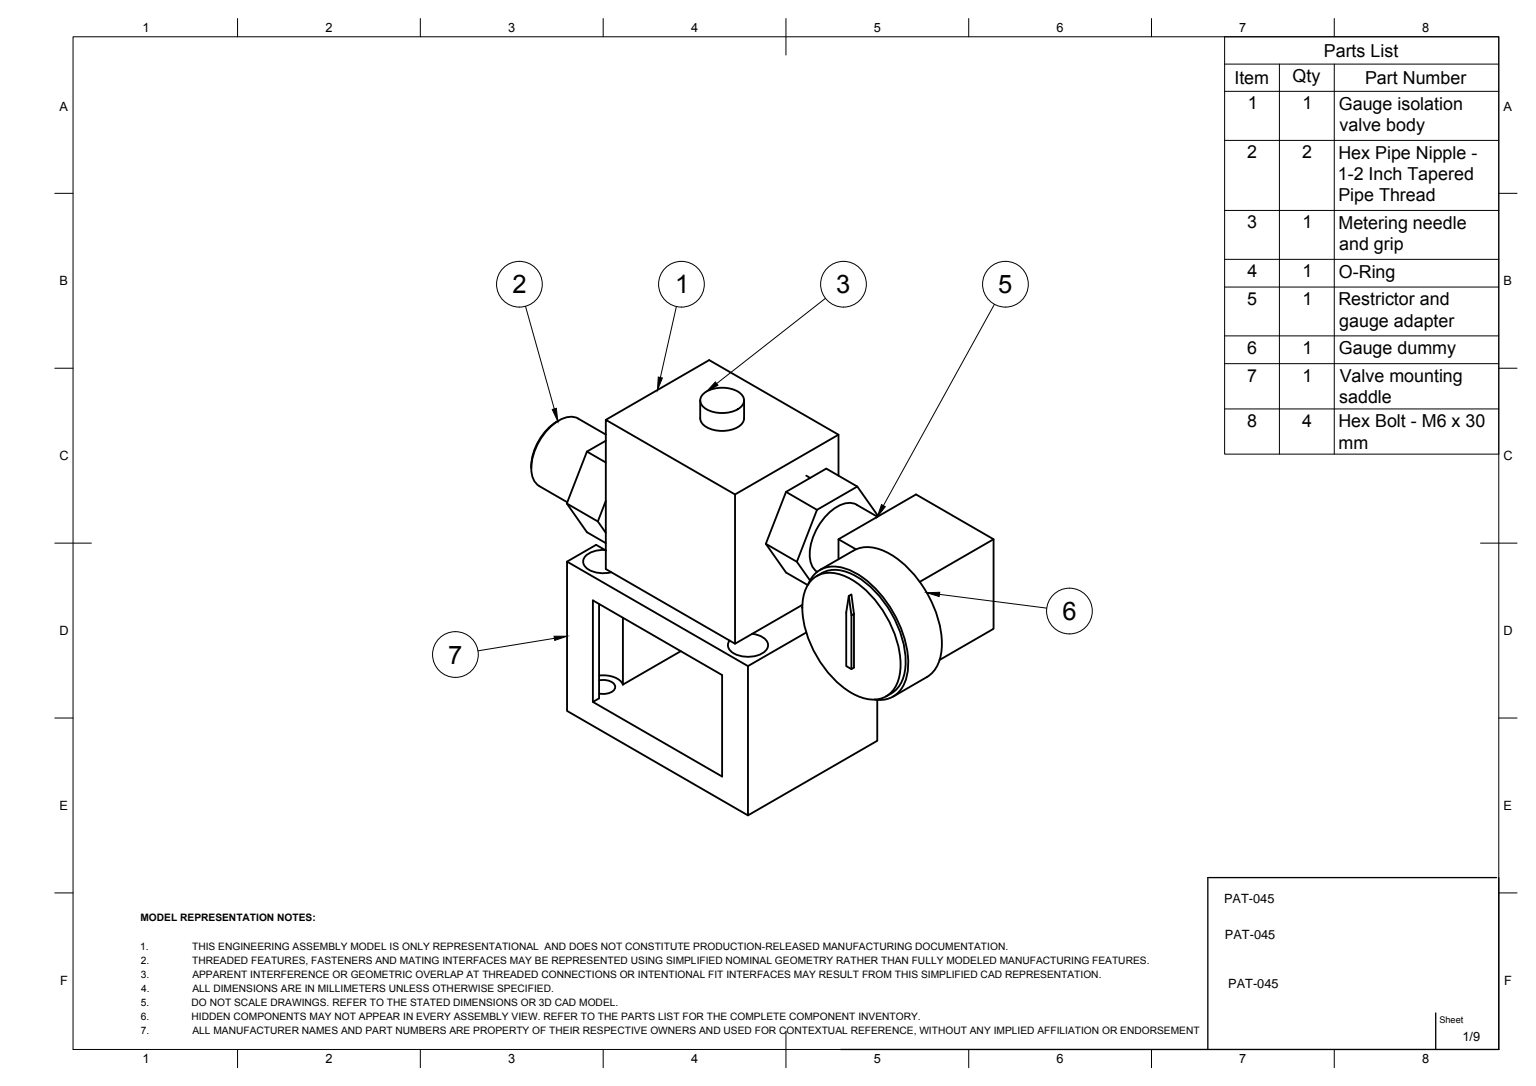
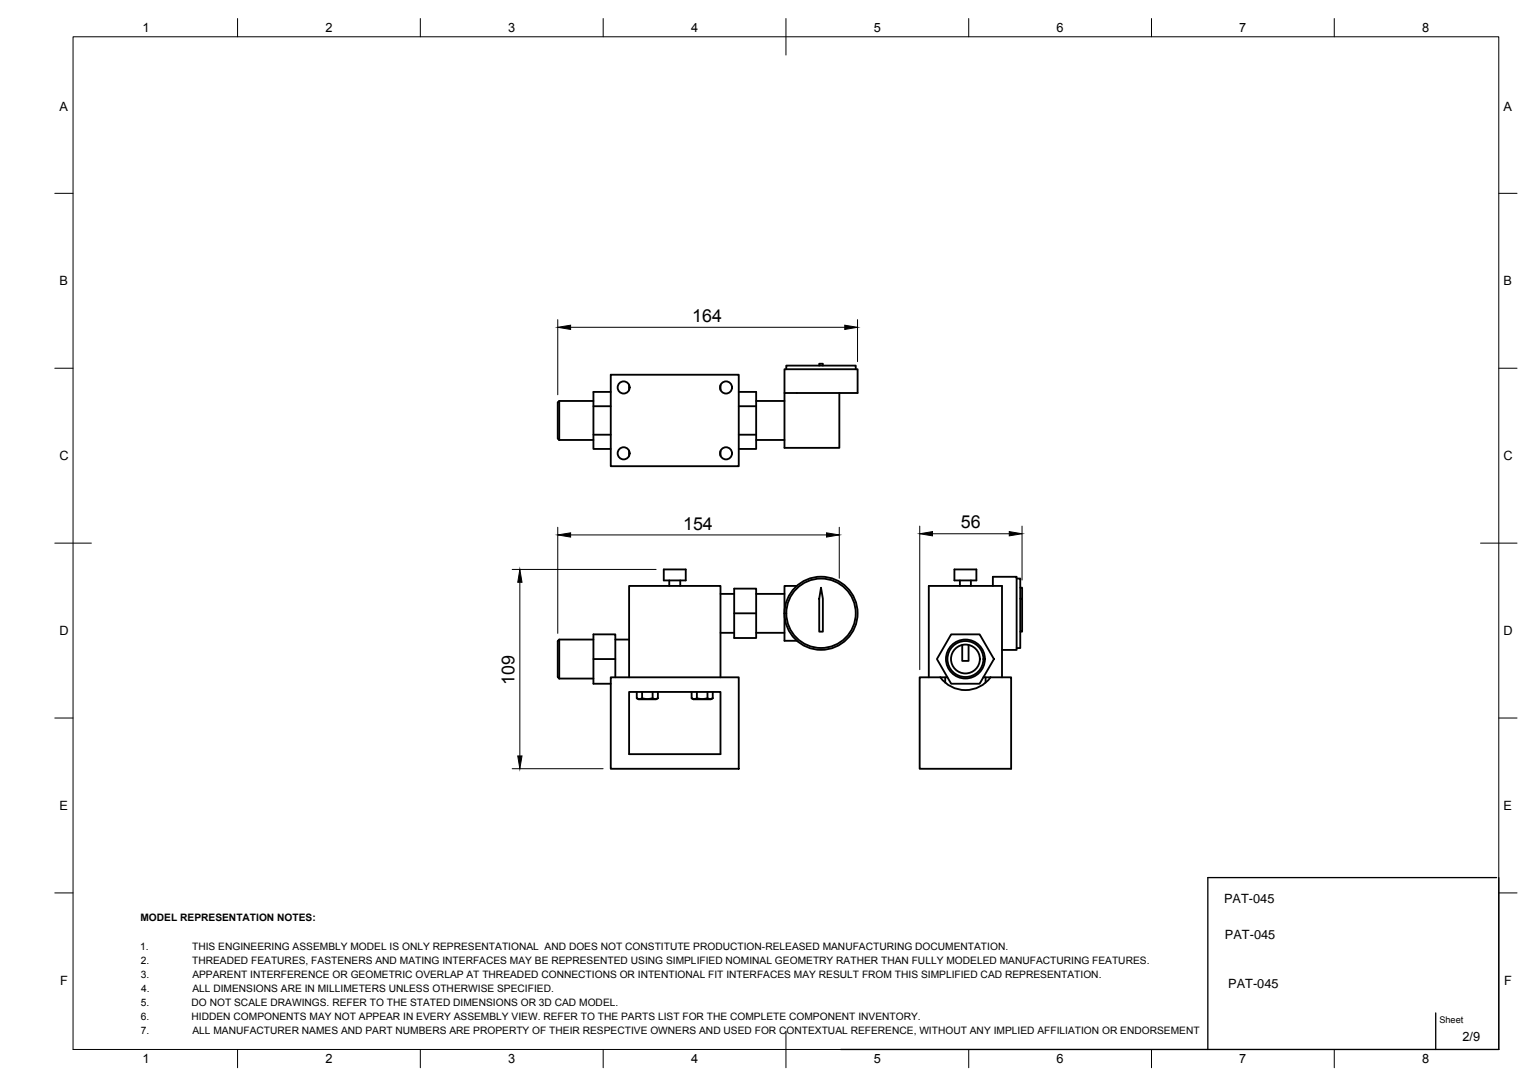
ISO-10303-21;
HEADER;
/* Generated by software containing ST-Developer
 * from STEP Tools, Inc. (www.steptools.com) 
 */

FILE_DESCRIPTION(
/* description */ ('Gauge isolation and snubber set'),
/* implementation_level */ '2;1');

FILE_NAME(
/* name */ 'PAT-045',
/* time_stamp */ '2026-10-29T16:58:15-07:00',
/* author */ (''),
/* organization */ (''),
/* preprocessor_version */ 'ST-DEVELOPER v20.2',
/* originating_system */ 'Autodesk Translation Framework v15.17.0.0',
/* authorisation */ '');

FILE_SCHEMA (('AUTOMOTIVE_DESIGN { 1 0 10303 214 3 1 1 }'));
ENDSEC;

DATA;
#10=MECHANICAL_DESIGN_GEOMETRIC_PRESENTATION_REPRESENTATION('',(#92,#93,
#94,#95,#96,#97,#98,#99,#100,#101),#4043);
#11=ITEM_DEFINED_TRANSFORMATION($,$,#2310,#2546);
#12=ITEM_DEFINED_TRANSFORMATION($,$,#2379,#2547);
#13=ITEM_DEFINED_TRANSFORMATION($,$,#2400,#2548);
#14=ITEM_DEFINED_TRANSFORMATION($,$,#2467,#2549);
#15=ITEM_DEFINED_TRANSFORMATION($,$,#2467,#2550);
#16=ITEM_DEFINED_TRANSFORMATION($,$,#2491,#2551);
#17=ITEM_DEFINED_TRANSFORMATION($,$,#2503,#2552);
#18=ITEM_DEFINED_TRANSFORMATION($,$,#2507,#2553);
#19=ITEM_DEFINED_TRANSFORMATION($,$,#2529,#2554);
#20=ITEM_DEFINED_TRANSFORMATION($,$,#2529,#2555);
#21=ITEM_DEFINED_TRANSFORMATION($,$,#2529,#2556);
#22=ITEM_DEFINED_TRANSFORMATION($,$,#2529,#2557);
#23=ITEM_DEFINED_TRANSFORMATION($,$,#2309,#2558);
#24=(
REPRESENTATION_RELATIONSHIP($,$,#4083,#4082)
REPRESENTATION_RELATIONSHIP_WITH_TRANSFORMATION(#11)
SHAPE_REPRESENTATION_RELATIONSHIP()
);
#25=(
REPRESENTATION_RELATIONSHIP($,$,#4084,#4082)
REPRESENTATION_RELATIONSHIP_WITH_TRANSFORMATION(#12)
SHAPE_REPRESENTATION_RELATIONSHIP()
);
#26=(
REPRESENTATION_RELATIONSHIP($,$,#4085,#4082)
REPRESENTATION_RELATIONSHIP_WITH_TRANSFORMATION(#13)
SHAPE_REPRESENTATION_RELATIONSHIP()
);
#27=(
REPRESENTATION_RELATIONSHIP($,$,#4086,#4082)
REPRESENTATION_RELATIONSHIP_WITH_TRANSFORMATION(#14)
SHAPE_REPRESENTATION_RELATIONSHIP()
);
#28=(
REPRESENTATION_RELATIONSHIP($,$,#4086,#4082)
REPRESENTATION_RELATIONSHIP_WITH_TRANSFORMATION(#15)
SHAPE_REPRESENTATION_RELATIONSHIP()
);
#29=(
REPRESENTATION_RELATIONSHIP($,$,#4087,#4082)
REPRESENTATION_RELATIONSHIP_WITH_TRANSFORMATION(#16)
SHAPE_REPRESENTATION_RELATIONSHIP()
);
#30=(
REPRESENTATION_RELATIONSHIP($,$,#4088,#4082)
REPRESENTATION_RELATIONSHIP_WITH_TRANSFORMATION(#17)
SHAPE_REPRESENTATION_RELATIONSHIP()
);
#31=(
REPRESENTATION_RELATIONSHIP($,$,#4089,#4082)
REPRESENTATION_RELATIONSHIP_WITH_TRANSFORMATION(#18)
SHAPE_REPRESENTATION_RELATIONSHIP()
);
#32=(
REPRESENTATION_RELATIONSHIP($,$,#4090,#4082)
REPRESENTATION_RELATIONSHIP_WITH_TRANSFORMATION(#19)
SHAPE_REPRESENTATION_RELATIONSHIP()
);
#33=(
REPRESENTATION_RELATIONSHIP($,$,#4090,#4082)
REPRESENTATION_RELATIONSHIP_WITH_TRANSFORMATION(#20)
SHAPE_REPRESENTATION_RELATIONSHIP()
);
#34=(
REPRESENTATION_RELATIONSHIP($,$,#4090,#4082)
REPRESENTATION_RELATIONSHIP_WITH_TRANSFORMATION(#21)
SHAPE_REPRESENTATION_RELATIONSHIP()
);
#35=(
REPRESENTATION_RELATIONSHIP($,$,#4090,#4082)
REPRESENTATION_RELATIONSHIP_WITH_TRANSFORMATION(#22)
SHAPE_REPRESENTATION_RELATIONSHIP()
);
#36=(
REPRESENTATION_RELATIONSHIP($,$,#4082,#4081)
REPRESENTATION_RELATIONSHIP_WITH_TRANSFORMATION(#23)
SHAPE_REPRESENTATION_RELATIONSHIP()
);
#37=CONTEXT_DEPENDENT_SHAPE_REPRESENTATION(#24,#4068);
#38=CONTEXT_DEPENDENT_SHAPE_REPRESENTATION(#25,#4069);
#39=CONTEXT_DEPENDENT_SHAPE_REPRESENTATION(#26,#4070);
#40=CONTEXT_DEPENDENT_SHAPE_REPRESENTATION(#27,#4071);
#41=CONTEXT_DEPENDENT_SHAPE_REPRESENTATION(#28,#4072);
#42=CONTEXT_DEPENDENT_SHAPE_REPRESENTATION(#29,#4073);
#43=CONTEXT_DEPENDENT_SHAPE_REPRESENTATION(#30,#4074);
#44=CONTEXT_DEPENDENT_SHAPE_REPRESENTATION(#31,#4075);
#45=CONTEXT_DEPENDENT_SHAPE_REPRESENTATION(#32,#4076);
#46=CONTEXT_DEPENDENT_SHAPE_REPRESENTATION(#33,#4077);
#47=CONTEXT_DEPENDENT_SHAPE_REPRESENTATION(#34,#4078);
#48=CONTEXT_DEPENDENT_SHAPE_REPRESENTATION(#35,#4079);
#49=CONTEXT_DEPENDENT_SHAPE_REPRESENTATION(#36,#4080);
#50=NEXT_ASSEMBLY_USAGE_OCCURRENCE('Gauge isolation valve body:1',
'Gauge isolation valve body:1','Gauge isolation valve body:1',#4093,#4094,
'Gauge isolation valve body:1');
#51=NEXT_ASSEMBLY_USAGE_OCCURRENCE('Restrictor and gauge adapter:1',
'Restrictor and gauge adapter:1','Restrictor and gauge adapter:1',#4093,
#4095,'Restrictor and gauge adapter:1');
#52=NEXT_ASSEMBLY_USAGE_OCCURRENCE('Valve mounting saddle:1',
'Valve mounting saddle:1','Valve mounting saddle:1',#4093,#4096,
'Valve mounting saddle:1');
#53=NEXT_ASSEMBLY_USAGE_OCCURRENCE(
'Hex Pipe Nipple - 1-2 Inch Tapered Pipe Thread:2',
'Hex Pipe Nipple - 1-2 Inch Tapered Pipe Thread:2',
'Hex Pipe Nipple - 1-2 Inch Tapered Pipe Thread:2',#4093,#4097,
'Hex Pipe Nipple - 1-2 Inch Tapered Pipe Thread:2');
#54=NEXT_ASSEMBLY_USAGE_OCCURRENCE(
'Hex Pipe Nipple - 1-2 Inch Tapered Pipe Thread:3',
'Hex Pipe Nipple - 1-2 Inch Tapered Pipe Thread:3',
'Hex Pipe Nipple - 1-2 Inch Tapered Pipe Thread:3',#4093,#4097,
'Hex Pipe Nipple - 1-2 Inch Tapered Pipe Thread:3');
#55=NEXT_ASSEMBLY_USAGE_OCCURRENCE('Metering needle and grip:2',
'Metering needle and grip:2','Metering needle and grip:2',#4093,#4098,
'Metering needle and grip:2');
#56=NEXT_ASSEMBLY_USAGE_OCCURRENCE('O-Ring:2','O-Ring:2','O-Ring:2',#4093,
#4099,'O-Ring:2');
#57=NEXT_ASSEMBLY_USAGE_OCCURRENCE('Gauge dummy:2','Gauge dummy:2',
'Gauge dummy:2',#4093,#4100,'Gauge dummy:2');
#58=NEXT_ASSEMBLY_USAGE_OCCURRENCE('Hex Bolt - M6 x 30 mm:2',
'Hex Bolt - M6 x 30 mm:2','Hex Bolt - M6 x 30 mm:2',#4093,#4101,
'Hex Bolt - M6 x 30 mm:2');
#59=NEXT_ASSEMBLY_USAGE_OCCURRENCE('Hex Bolt - M6 x 30 mm:3',
'Hex Bolt - M6 x 30 mm:3','Hex Bolt - M6 x 30 mm:3',#4093,#4101,
'Hex Bolt - M6 x 30 mm:3');
#60=NEXT_ASSEMBLY_USAGE_OCCURRENCE('Hex Bolt - M6 x 30 mm:4',
'Hex Bolt - M6 x 30 mm:4','Hex Bolt - M6 x 30 mm:4',#4093,#4101,
'Hex Bolt - M6 x 30 mm:4');
#61=NEXT_ASSEMBLY_USAGE_OCCURRENCE('Hex Bolt - M6 x 30 mm:5',
'Hex Bolt - M6 x 30 mm:5','Hex Bolt - M6 x 30 mm:5',#4093,#4101,
'Hex Bolt - M6 x 30 mm:5');
#62=NEXT_ASSEMBLY_USAGE_OCCURRENCE('Guage isolation set:1',
'Guage isolation set:1','Guage isolation set:1',#4092,#4093,
'Guage isolation set:1');
#63=(
BOUNDED_CURVE()
B_SPLINE_CURVE(2,(#3961,#3962,#3963),.UNSPECIFIED.,.F.,.F.)
B_SPLINE_CURVE_WITH_KNOTS((3,3),(0.144988513094728,0.791574906712449),
 .UNSPECIFIED.)
CURVE()
GEOMETRIC_REPRESENTATION_ITEM()
RATIONAL_B_SPLINE_CURVE((1.09282032302755,1.26188021535082,1.09282032302931))
REPRESENTATION_ITEM('')
);
#64=(
BOUNDED_CURVE()
B_SPLINE_CURVE(2,(#3965,#3966,#3967),.UNSPECIFIED.,.F.,.F.)
B_SPLINE_CURVE_WITH_KNOTS((3,3),(0.144988513094728,0.791574906712449),
 .UNSPECIFIED.)
CURVE()
GEOMETRIC_REPRESENTATION_ITEM()
RATIONAL_B_SPLINE_CURVE((1.09282032302755,1.26188021535082,1.09282032302931))
REPRESENTATION_ITEM('')
);
#65=(
BOUNDED_CURVE()
B_SPLINE_CURVE(2,(#3969,#3970,#3971),.UNSPECIFIED.,.F.,.F.)
B_SPLINE_CURVE_WITH_KNOTS((3,3),(0.144988513094728,0.791574906712449),
 .UNSPECIFIED.)
CURVE()
GEOMETRIC_REPRESENTATION_ITEM()
RATIONAL_B_SPLINE_CURVE((1.09282032302755,1.26188021535082,1.09282032302931))
REPRESENTATION_ITEM('')
);
#66=(
BOUNDED_CURVE()
B_SPLINE_CURVE(2,(#3973,#3974,#3975),.UNSPECIFIED.,.F.,.F.)
B_SPLINE_CURVE_WITH_KNOTS((3,3),(0.144988513094728,0.791574906712449),
 .UNSPECIFIED.)
CURVE()
GEOMETRIC_REPRESENTATION_ITEM()
RATIONAL_B_SPLINE_CURVE((1.09282032302755,1.26188021535082,1.09282032302931))
REPRESENTATION_ITEM('')
);
#67=(
BOUNDED_CURVE()
B_SPLINE_CURVE(2,(#3977,#3978,#3979),.UNSPECIFIED.,.F.,.F.)
B_SPLINE_CURVE_WITH_KNOTS((3,3),(0.144988513094728,0.791574906712449),
 .UNSPECIFIED.)
CURVE()
GEOMETRIC_REPRESENTATION_ITEM()
RATIONAL_B_SPLINE_CURVE((1.09282032302755,1.26188021535082,1.09282032302931))
REPRESENTATION_ITEM('')
);
#68=(
BOUNDED_CURVE()
B_SPLINE_CURVE(2,(#3980,#3981,#3982),.UNSPECIFIED.,.F.,.F.)
B_SPLINE_CURVE_WITH_KNOTS((3,3),(0.144988513094727,0.791574906712449),
 .UNSPECIFIED.)
CURVE()
GEOMETRIC_REPRESENTATION_ITEM()
RATIONAL_B_SPLINE_CURVE((1.09282032302755,1.26188021535082,1.09282032302931))
REPRESENTATION_ITEM('')
);
#69=TOROIDAL_SURFACE('',#2504,0.3925,0.089);
#70=CONICAL_SURFACE('',#2483,1.025,0.785398163397448);
#71=CONICAL_SURFACE('',#2486,1.025,0.785398163397448);
#72=CONICAL_SURFACE('',#2492,0.1,0.78539816339745);
#73=CONICAL_SURFACE('',#2494,0.25,0.321750554396641);
#74=CONICAL_SURFACE('',#2533,0.27,0.785398163397448);
#75=CONICAL_SURFACE('',#2536,0.576175134594813,1.0471975511966);
#76=SHAPE_REPRESENTATION_RELATIONSHIP('SRR','None',#4083,#84);
#77=SHAPE_REPRESENTATION_RELATIONSHIP('SRR','None',#4084,#85);
#78=SHAPE_REPRESENTATION_RELATIONSHIP('SRR','None',#4085,#86);
#79=SHAPE_REPRESENTATION_RELATIONSHIP('SRR','None',#4086,#87);
#80=SHAPE_REPRESENTATION_RELATIONSHIP('SRR','None',#4087,#88);
#81=SHAPE_REPRESENTATION_RELATIONSHIP('SRR','None',#4088,#89);
#82=SHAPE_REPRESENTATION_RELATIONSHIP('SRR','None',#4089,#90);
#83=SHAPE_REPRESENTATION_RELATIONSHIP('SRR','None',#4090,#91);
#84=ADVANCED_BREP_SHAPE_REPRESENTATION('',(#102),#4035);
#85=ADVANCED_BREP_SHAPE_REPRESENTATION('',(#103),#4036);
#86=ADVANCED_BREP_SHAPE_REPRESENTATION('',(#104),#4037);
#87=ADVANCED_BREP_SHAPE_REPRESENTATION('',(#105),#4038);
#88=ADVANCED_BREP_SHAPE_REPRESENTATION('',(#106),#4039);
#89=ADVANCED_BREP_SHAPE_REPRESENTATION('',(#107),#4040);
#90=ADVANCED_BREP_SHAPE_REPRESENTATION('',(#108,#109,#110),#4041);
#91=ADVANCED_BREP_SHAPE_REPRESENTATION('',(#111),#4042);
#92=STYLED_ITEM('',(#4176),#102);
#93=STYLED_ITEM('',(#4183),#103);
#94=STYLED_ITEM('',(#4211),#104);
#95=STYLED_ITEM('',(#4183),#105);
#96=STYLED_ITEM('',(#4204),#106);
#97=STYLED_ITEM('',(#4204),#107);
#98=STYLED_ITEM('',(#4211),#108);
#99=STYLED_ITEM('',(#4211),#109);
#100=STYLED_ITEM('',(#4211),#110);
#101=STYLED_ITEM('',(#4204),#111);
#102=MANIFOLD_SOLID_BREP('Body1',#2209);
#103=MANIFOLD_SOLID_BREP('Body1',#2210);
#104=MANIFOLD_SOLID_BREP('Body1',#2211);
#105=MANIFOLD_SOLID_BREP('Body1',#2212);
#106=MANIFOLD_SOLID_BREP('Body1',#2213);
#107=MANIFOLD_SOLID_BREP('Body1',#2214);
#108=MANIFOLD_SOLID_BREP('Body1',#2215);
#109=MANIFOLD_SOLID_BREP('Off white dial',#2216);
#110=MANIFOLD_SOLID_BREP('Black pointer',#2217);
#111=MANIFOLD_SOLID_BREP('Body1',#2218);
#112=FACE_BOUND('',#379,.T.);
#113=FACE_BOUND('',#382,.T.);
#114=FACE_BOUND('',#384,.T.);
#115=FACE_BOUND('',#389,.T.);
#116=FACE_BOUND('',#397,.T.);
#117=FACE_BOUND('',#400,.T.);
#118=FACE_BOUND('',#403,.T.);
#119=FACE_BOUND('',#405,.T.);
#120=FACE_BOUND('',#407,.T.);
#121=FACE_BOUND('',#408,.T.);
#122=FACE_BOUND('',#409,.T.);
#123=FACE_BOUND('',#410,.T.);
#124=FACE_BOUND('',#415,.T.);
#125=FACE_BOUND('',#419,.T.);
#126=FACE_BOUND('',#423,.T.);
#127=FACE_BOUND('',#425,.T.);
#128=FACE_BOUND('',#436,.T.);
#129=FACE_BOUND('',#437,.T.);
#130=FACE_BOUND('',#438,.T.);
#131=FACE_BOUND('',#439,.T.);
#132=FACE_BOUND('',#442,.T.);
#133=FACE_BOUND('',#443,.T.);
#134=FACE_BOUND('',#444,.T.);
#135=FACE_BOUND('',#445,.T.);
#136=FACE_BOUND('',#460,.T.);
#137=FACE_BOUND('',#462,.T.);
#138=FACE_BOUND('',#463,.T.);
#139=FACE_BOUND('',#464,.T.);
#140=FACE_BOUND('',#465,.T.);
#141=FACE_BOUND('',#467,.T.);
#142=FACE_BOUND('',#470,.T.);
#143=FACE_BOUND('',#471,.T.);
#144=FACE_BOUND('',#472,.T.);
#145=FACE_BOUND('',#473,.T.);
#146=FACE_BOUND('',#475,.T.);
#147=FACE_BOUND('',#477,.T.);
#148=FACE_BOUND('',#486,.T.);
#149=FACE_BOUND('',#491,.T.);
#150=FACE_BOUND('',#497,.T.);
#151=FACE_BOUND('',#502,.T.);
#152=FACE_BOUND('',#529,.T.);
#153=B_SPLINE_CURVE_WITH_KNOTS('',3,(#3286,#3287,#3288,#3289,#3290,#3291,
#3292,#3293,#3294,#3295,#3296,#3297,#3298,#3299,#3300,#3301,#3302,#3303),
 .UNSPECIFIED.,.F.,.F.,(4,2,2,2,2,2,2,2,4),(0.,0.0769830401762947,0.153966080352589,
0.230739261017803,0.307512441683016,0.384285622348229,0.461058803013443,
0.538041843189737,0.615024883366032),.UNSPECIFIED.);
#154=B_SPLINE_CURVE_WITH_KNOTS('',3,(#3360,#3361,#3362,#3363,#3364,#3365,
#3366,#3367,#3368,#3369,#3370,#3371,#3372,#3373,#3374),.UNSPECIFIED.,.F.,
 .F.,(4,2,2,2,3,2,4),(-0.302773934408822,-0.227086024595877,-0.151398114782933,
-0.0756990573914662,0.,0.0756990573914663,0.1003787904191),
 .UNSPECIFIED.);
#155=B_SPLINE_CURVE_WITH_KNOTS('',3,(#3377,#3378,#3379,#3380,#3381,#3382,
#3383,#3384,#3385,#3386,#3387,#3388,#3389,#3390),.UNSPECIFIED.,.F.,.F.,
(4,2,2,2,2,2,4),(-0.705926659236745,-0.681246926209111,-0.605547868817645,
-0.529848811426178,-0.454149754034712,-0.378461844221767,-0.302773934408822),
 .UNSPECIFIED.);
#156=B_SPLINE_CURVE_WITH_KNOTS('',3,(#3445,#3446,#3447,#3448,#3449,#3450,
#3451,#3452,#3453,#3454),.UNSPECIFIED.,.F.,.F.,(4,2,2,2,4),(0.0753445150177796,
0.0847625796770749,0.0941806443363702,0.10359870843152,0.113016772526669),
 .UNSPECIFIED.);
#157=B_SPLINE_CURVE_WITH_KNOTS('',3,(#3456,#3457,#3458,#3459,#3460,#3461,
#3462,#3463,#3464,#3465),.UNSPECIFIED.,.F.,.F.,(4,2,2,2,4),(0.0376722575088898,
0.0470903216040394,0.056508385699189,0.0659264503584843,0.0753445150177796),
 .UNSPECIFIED.);
#158=B_SPLINE_CURVE_WITH_KNOTS('',3,(#3470,#3471,#3472,#3473,#3474,#3475,
#3476,#3477,#3478,#3479),.UNSPECIFIED.,.F.,.F.,(4,2,2,2,4),(0.,0.0094180646592953,
0.0188361293185906,0.0282541934137402,0.0376722575088898),.UNSPECIFIED.);
#159=B_SPLINE_CURVE_WITH_KNOTS('',3,(#3480,#3481,#3482,#3483,#3484,#3485,
#3486,#3487,#3488,#3489),.UNSPECIFIED.,.F.,.F.,(4,2,2,2,4),(0.113016772526669,
0.122434836621819,0.131852900716969,0.141270965376264,0.150689030035559),
 .UNSPECIFIED.);
#160=B_SPLINE_CURVE_WITH_KNOTS('',3,(#3540,#3541,#3542,#3543,#3544,#3545,
#3546,#3547,#3548,#3549,#3550,#3551,#3552,#3553,#3554,#3555,#3556,#3557,
#3558,#3559),.UNSPECIFIED.,.F.,.F.,(4,2,2,2,2,2,2,2,2,4),(2.69569624904958,
2.75192095998156,2.89158432667083,3.02781992201341,3.15222641361202,3.27663290521063,
3.40103939680924,3.52544588840784,3.66168148375042,3.68881758098469),
 .UNSPECIFIED.);
#161=B_SPLINE_CURVE_WITH_KNOTS('',3,(#3563,#3564,#3565,#3566,#3567,#3568,
#3569,#3570,#3571,#3572,#3573,#3574,#3575,#3576),.UNSPECIFIED.,.F.,.F.,
(4,2,2,2,2,2,4),(2.49458037721665,2.67223802177451,2.78657360475194,2.90090918772936,
3.01524477070679,3.12958035368422,3.30723799824207),.UNSPECIFIED.);
#162=B_SPLINE_CURVE_WITH_KNOTS('',3,(#3584,#3585,#3586,#3587,#3588,#3589,
#3590,#3591,#3592,#3593,#3594,#3595,#3596,#3597,#3598),.UNSPECIFIED.,.F.,
 .F.,(4,2,2,3,2,2,4),(-0.40632881051271,-0.228671165954853,-0.114335582977427,
0.,0.114335582977426,0.228671165954853,0.40632881051271),.UNSPECIFIED.);
#163=B_SPLINE_CURVE_WITH_KNOTS('',3,(#3601,#3602,#3603,#3604,#3605,#3606,
#3607,#3608,#3609,#3610,#3611,#3612,#3613,#3614,#3615,#3616,#3617,#3618,
#3619,#3620,#3621),.UNSPECIFIED.,.F.,.F.,(4,2,2,2,3,2,2,2,2,4),(-0.412184675816244,
-0.385048578539797,-0.248812983197217,-0.124406491598609,0.,0.124406491598609,
0.248812983197217,0.385048578539798,0.524711945229068,0.58093665616105),
 .UNSPECIFIED.);
#164=PLANE('',#2319);
#165=PLANE('',#2323);
#166=PLANE('',#2327);
#167=PLANE('',#2331);
#168=PLANE('',#2332);
#169=PLANE('',#2339);
#170=PLANE('',#2343);
#171=PLANE('',#2347);
#172=PLANE('',#2349);
#173=PLANE('',#2358);
#174=PLANE('',#2359);
#175=PLANE('',#2362);
#176=PLANE('',#2365);
#177=PLANE('',#2372);
#178=PLANE('',#2373);
#179=PLANE('',#2374);
#180=PLANE('',#2375);
#181=PLANE('',#2376);
#182=PLANE('',#2377);
#183=PLANE('',#2378);
#184=PLANE('',#2383);
#185=PLANE('',#2387);
#186=PLANE('',#2393);
#187=PLANE('',#2394);
#188=PLANE('',#2395);
#189=PLANE('',#2396);
#190=PLANE('',#2397);
#191=PLANE('',#2398);
#192=PLANE('',#2399);
#193=PLANE('',#2401);
#194=PLANE('',#2424);
#195=PLANE('',#2425);
#196=PLANE('',#2435);
#197=PLANE('',#2443);
#198=PLANE('',#2446);
#199=PLANE('',#2447);
#200=PLANE('',#2450);
#201=PLANE('',#2456);
#202=PLANE('',#2461);
#203=PLANE('',#2462);
#204=PLANE('',#2463);
#205=PLANE('',#2464);
#206=PLANE('',#2465);
#207=PLANE('',#2466);
#208=PLANE('',#2468);
#209=PLANE('',#2470);
#210=PLANE('',#2472);
#211=PLANE('',#2473);
#212=PLANE('',#2474);
#213=PLANE('',#2475);
#214=PLANE('',#2476);
#215=PLANE('',#2477);
#216=PLANE('',#2480);
#217=PLANE('',#2488);
#218=PLANE('',#2498);
#219=PLANE('',#2502);
#220=PLANE('',#2508);
#221=PLANE('',#2513);
#222=PLANE('',#2516);
#223=PLANE('',#2520);
#224=PLANE('',#2521);
#225=PLANE('',#2522);
#226=PLANE('',#2523);
#227=PLANE('',#2524);
#228=PLANE('',#2525);
#229=PLANE('',#2526);
#230=PLANE('',#2527);
#231=PLANE('',#2528);
#232=PLANE('',#2535);
#233=PLANE('',#2538);
#234=PLANE('',#2539);
#235=PLANE('',#2540);
#236=PLANE('',#2541);
#237=PLANE('',#2542);
#238=PLANE('',#2543);
#239=PLANE('',#2544);
#240=PLANE('',#2545);
#241=FACE_OUTER_BOUND('',#365,.T.);
#242=FACE_OUTER_BOUND('',#366,.T.);
#243=FACE_OUTER_BOUND('',#367,.T.);
#244=FACE_OUTER_BOUND('',#368,.T.);
#245=FACE_OUTER_BOUND('',#369,.T.);
#246=FACE_OUTER_BOUND('',#370,.T.);
#247=FACE_OUTER_BOUND('',#371,.T.);
#248=FACE_OUTER_BOUND('',#372,.T.);
#249=FACE_OUTER_BOUND('',#373,.T.);
#250=FACE_OUTER_BOUND('',#374,.T.);
#251=FACE_OUTER_BOUND('',#375,.T.);
#252=FACE_OUTER_BOUND('',#376,.T.);
#253=FACE_OUTER_BOUND('',#377,.T.);
#254=FACE_OUTER_BOUND('',#378,.T.);
#255=FACE_OUTER_BOUND('',#380,.T.);
#256=FACE_OUTER_BOUND('',#381,.T.);
#257=FACE_OUTER_BOUND('',#383,.T.);
#258=FACE_OUTER_BOUND('',#385,.T.);
#259=FACE_OUTER_BOUND('',#386,.T.);
#260=FACE_OUTER_BOUND('',#387,.T.);
#261=FACE_OUTER_BOUND('',#388,.T.);
#262=FACE_OUTER_BOUND('',#390,.T.);
#263=FACE_OUTER_BOUND('',#391,.T.);
#264=FACE_OUTER_BOUND('',#392,.T.);
#265=FACE_OUTER_BOUND('',#393,.T.);
#266=FACE_OUTER_BOUND('',#394,.T.);
#267=FACE_OUTER_BOUND('',#395,.T.);
#268=FACE_OUTER_BOUND('',#396,.T.);
#269=FACE_OUTER_BOUND('',#398,.T.);
#270=FACE_OUTER_BOUND('',#399,.T.);
#271=FACE_OUTER_BOUND('',#401,.T.);
#272=FACE_OUTER_BOUND('',#402,.T.);
#273=FACE_OUTER_BOUND('',#404,.T.);
#274=FACE_OUTER_BOUND('',#406,.T.);
#275=FACE_OUTER_BOUND('',#411,.T.);
#276=FACE_OUTER_BOUND('',#412,.T.);
#277=FACE_OUTER_BOUND('',#413,.T.);
#278=FACE_OUTER_BOUND('',#414,.T.);
#279=FACE_OUTER_BOUND('',#416,.T.);
#280=FACE_OUTER_BOUND('',#417,.T.);
#281=FACE_OUTER_BOUND('',#418,.T.);
#282=FACE_OUTER_BOUND('',#420,.T.);
#283=FACE_OUTER_BOUND('',#421,.T.);
#284=FACE_OUTER_BOUND('',#422,.T.);
#285=FACE_OUTER_BOUND('',#424,.T.);
#286=FACE_OUTER_BOUND('',#426,.T.);
#287=FACE_OUTER_BOUND('',#427,.T.);
#288=FACE_OUTER_BOUND('',#428,.T.);
#289=FACE_OUTER_BOUND('',#429,.T.);
#290=FACE_OUTER_BOUND('',#430,.T.);
#291=FACE_OUTER_BOUND('',#431,.T.);
#292=FACE_OUTER_BOUND('',#432,.T.);
#293=FACE_OUTER_BOUND('',#433,.T.);
#294=FACE_OUTER_BOUND('',#434,.T.);
#295=FACE_OUTER_BOUND('',#435,.T.);
#296=FACE_OUTER_BOUND('',#440,.T.);
#297=FACE_OUTER_BOUND('',#441,.T.);
#298=FACE_OUTER_BOUND('',#446,.T.);
#299=FACE_OUTER_BOUND('',#447,.T.);
#300=FACE_OUTER_BOUND('',#448,.T.);
#301=FACE_OUTER_BOUND('',#449,.T.);
#302=FACE_OUTER_BOUND('',#450,.T.);
#303=FACE_OUTER_BOUND('',#451,.T.);
#304=FACE_OUTER_BOUND('',#452,.T.);
#305=FACE_OUTER_BOUND('',#453,.T.);
#306=FACE_OUTER_BOUND('',#454,.T.);
#307=FACE_OUTER_BOUND('',#455,.T.);
#308=FACE_OUTER_BOUND('',#456,.T.);
#309=FACE_OUTER_BOUND('',#457,.T.);
#310=FACE_OUTER_BOUND('',#458,.T.);
#311=FACE_OUTER_BOUND('',#459,.T.);
#312=FACE_OUTER_BOUND('',#461,.T.);
#313=FACE_OUTER_BOUND('',#466,.T.);
#314=FACE_OUTER_BOUND('',#468,.T.);
#315=FACE_OUTER_BOUND('',#469,.T.);
#316=FACE_OUTER_BOUND('',#474,.T.);
#317=FACE_OUTER_BOUND('',#476,.T.);
#318=FACE_OUTER_BOUND('',#478,.T.);
#319=FACE_OUTER_BOUND('',#479,.T.);
#320=FACE_OUTER_BOUND('',#480,.T.);
#321=FACE_OUTER_BOUND('',#481,.T.);
#322=FACE_OUTER_BOUND('',#482,.T.);
#323=FACE_OUTER_BOUND('',#483,.T.);
#324=FACE_OUTER_BOUND('',#484,.T.);
#325=FACE_OUTER_BOUND('',#485,.T.);
#326=FACE_OUTER_BOUND('',#487,.T.);
#327=FACE_OUTER_BOUND('',#488,.T.);
#328=FACE_OUTER_BOUND('',#489,.T.);
#329=FACE_OUTER_BOUND('',#490,.T.);
#330=FACE_OUTER_BOUND('',#492,.T.);
#331=FACE_OUTER_BOUND('',#493,.T.);
#332=FACE_OUTER_BOUND('',#494,.T.);
#333=FACE_OUTER_BOUND('',#495,.T.);
#334=FACE_OUTER_BOUND('',#496,.T.);
#335=FACE_OUTER_BOUND('',#498,.T.);
#336=FACE_OUTER_BOUND('',#499,.T.);
#337=FACE_OUTER_BOUND('',#500,.T.);
#338=FACE_OUTER_BOUND('',#501,.T.);
#339=FACE_OUTER_BOUND('',#503,.T.);
#340=FACE_OUTER_BOUND('',#504,.T.);
#341=FACE_OUTER_BOUND('',#505,.T.);
#342=FACE_OUTER_BOUND('',#506,.T.);
#343=FACE_OUTER_BOUND('',#507,.T.);
#344=FACE_OUTER_BOUND('',#508,.T.);
#345=FACE_OUTER_BOUND('',#509,.T.);
#346=FACE_OUTER_BOUND('',#510,.T.);
#347=FACE_OUTER_BOUND('',#511,.T.);
#348=FACE_OUTER_BOUND('',#512,.T.);
#349=FACE_OUTER_BOUND('',#513,.T.);
#350=FACE_OUTER_BOUND('',#514,.T.);
#351=FACE_OUTER_BOUND('',#515,.T.);
#352=FACE_OUTER_BOUND('',#516,.T.);
#353=FACE_OUTER_BOUND('',#517,.T.);
#354=FACE_OUTER_BOUND('',#518,.T.);
#355=FACE_OUTER_BOUND('',#519,.T.);
#356=FACE_OUTER_BOUND('',#520,.T.);
#357=FACE_OUTER_BOUND('',#521,.T.);
#358=FACE_OUTER_BOUND('',#522,.T.);
#359=FACE_OUTER_BOUND('',#523,.T.);
#360=FACE_OUTER_BOUND('',#524,.T.);
#361=FACE_OUTER_BOUND('',#525,.T.);
#362=FACE_OUTER_BOUND('',#526,.T.);
#363=FACE_OUTER_BOUND('',#527,.T.);
#364=FACE_OUTER_BOUND('',#528,.T.);
#365=EDGE_LOOP('',(#1461,#1462,#1463,#1464,#1465));
#366=EDGE_LOOP('',(#1466,#1467,#1468,#1469));
#367=EDGE_LOOP('',(#1470));
#368=EDGE_LOOP('',(#1471,#1472,#1473,#1474));
#369=EDGE_LOOP('',(#1475));
#370=EDGE_LOOP('',(#1476,#1477,#1478,#1479));
#371=EDGE_LOOP('',(#1480));
#372=EDGE_LOOP('',(#1481,#1482,#1483,#1484));
#373=EDGE_LOOP('',(#1485));
#374=EDGE_LOOP('',(#1486,#1487,#1488));
#375=EDGE_LOOP('',(#1489,#1490,#1491,#1492,#1493,#1494,#1495,#1496,#1497,
#1498,#1499,#1500));
#376=EDGE_LOOP('',(#1501,#1502,#1503));
#377=EDGE_LOOP('',(#1504,#1505,#1506,#1507));
#378=EDGE_LOOP('',(#1508));
#379=EDGE_LOOP('',(#1509));
#380=EDGE_LOOP('',(#1510,#1511,#1512,#1513));
#381=EDGE_LOOP('',(#1514));
#382=EDGE_LOOP('',(#1515));
#383=EDGE_LOOP('',(#1516));
#384=EDGE_LOOP('',(#1517));
#385=EDGE_LOOP('',(#1518,#1519,#1520,#1521));
#386=EDGE_LOOP('',(#1522,#1523,#1524,#1525));
#387=EDGE_LOOP('',(#1526,#1527,#1528,#1529,#1530));
#388=EDGE_LOOP('',(#1531,#1532));
#389=EDGE_LOOP('',(#1533));
#390=EDGE_LOOP('',(#1534,#1535,#1536,#1537,#1538,#1539,#1540,#1541));
#391=EDGE_LOOP('',(#1542,#1543));
#392=EDGE_LOOP('',(#1544,#1545,#1546,#1547,#1548,#1549,#1550,#1551,#1552,
#1553,#1554,#1555));
#393=EDGE_LOOP('',(#1556,#1557,#1558,#1559));
#394=EDGE_LOOP('',(#1560,#1561,#1562,#1563,#1564,#1565));
#395=EDGE_LOOP('',(#1566,#1567,#1568,#1569));
#396=EDGE_LOOP('',(#1570));
#397=EDGE_LOOP('',(#1571));
#398=EDGE_LOOP('',(#1572,#1573,#1574,#1575));
#399=EDGE_LOOP('',(#1576,#1577,#1578,#1579));
#400=EDGE_LOOP('',(#1580));
#401=EDGE_LOOP('',(#1581,#1582,#1583,#1584));
#402=EDGE_LOOP('',(#1585,#1586,#1587,#1588));
#403=EDGE_LOOP('',(#1589));
#404=EDGE_LOOP('',(#1590,#1591,#1592,#1593));
#405=EDGE_LOOP('',(#1594));
#406=EDGE_LOOP('',(#1595,#1596,#1597,#1598));
#407=EDGE_LOOP('',(#1599));
#408=EDGE_LOOP('',(#1600));
#409=EDGE_LOOP('',(#1601));
#410=EDGE_LOOP('',(#1602));
#411=EDGE_LOOP('',(#1603,#1604,#1605,#1606));
#412=EDGE_LOOP('',(#1607));
#413=EDGE_LOOP('',(#1608,#1609,#1610,#1611,#1612,#1613,#1614,#1615,#1616,
#1617));
#414=EDGE_LOOP('',(#1618));
#415=EDGE_LOOP('',(#1619));
#416=EDGE_LOOP('',(#1620,#1621,#1622,#1623,#1624,#1625,#1626));
#417=EDGE_LOOP('',(#1627,#1628,#1629,#1630));
#418=EDGE_LOOP('',(#1631));
#419=EDGE_LOOP('',(#1632));
#420=EDGE_LOOP('',(#1633,#1634,#1635,#1636));
#421=EDGE_LOOP('',(#1637,#1638,#1639,#1640));
#422=EDGE_LOOP('',(#1641,#1642,#1643,#1644));
#423=EDGE_LOOP('',(#1645));
#424=EDGE_LOOP('',(#1646,#1647,#1648,#1649));
#425=EDGE_LOOP('',(#1650));
#426=EDGE_LOOP('',(#1651,#1652,#1653,#1654));
#427=EDGE_LOOP('',(#1655,#1656,#1657,#1658));
#428=EDGE_LOOP('',(#1659,#1660,#1661,#1662));
#429=EDGE_LOOP('',(#1663,#1664,#1665,#1666,#1667,#1668,#1669,#1670,#1671,
#1672));
#430=EDGE_LOOP('',(#1673,#1674,#1675,#1676,#1677,#1678,#1679,#1680,#1681,
#1682));
#431=EDGE_LOOP('',(#1683,#1684,#1685,#1686,#1687,#1688,#1689));
#432=EDGE_LOOP('',(#1690,#1691,#1692,#1693,#1694,#1695,#1696));
#433=EDGE_LOOP('',(#1697,#1698,#1699,#1700,#1701,#1702,#1703,#1704));
#434=EDGE_LOOP('',(#1705,#1706,#1707,#1708));
#435=EDGE_LOOP('',(#1709,#1710,#1711,#1712,#1713,#1714,#1715,#1716,#1717,
#1718,#1719,#1720,#1721,#1722));
#436=EDGE_LOOP('',(#1723));
#437=EDGE_LOOP('',(#1724));
#438=EDGE_LOOP('',(#1725));
#439=EDGE_LOOP('',(#1726));
#440=EDGE_LOOP('',(#1727,#1728,#1729,#1730));
#441=EDGE_LOOP('',(#1731,#1732,#1733,#1734,#1735,#1736,#1737,#1738,#1739,
#1740,#1741,#1742,#1743,#1744));
#442=EDGE_LOOP('',(#1745));
#443=EDGE_LOOP('',(#1746));
#444=EDGE_LOOP('',(#1747));
#445=EDGE_LOOP('',(#1748));
#446=EDGE_LOOP('',(#1749,#1750,#1751,#1752,#1753,#1754,#1755,#1756));
#447=EDGE_LOOP('',(#1757,#1758,#1759,#1760));
#448=EDGE_LOOP('',(#1761,#1762,#1763,#1764));
#449=EDGE_LOOP('',(#1765,#1766,#1767,#1768));
#450=EDGE_LOOP('',(#1769,#1770,#1771,#1772));
#451=EDGE_LOOP('',(#1773,#1774,#1775,#1776));
#452=EDGE_LOOP('',(#1777,#1778,#1779,#1780));
#453=EDGE_LOOP('',(#1781,#1782,#1783,#1784,#1785,#1786,#1787,#1788,#1789,
#1790));
#454=EDGE_LOOP('',(#1791,#1792,#1793,#1794));
#455=EDGE_LOOP('',(#1795,#1796,#1797,#1798));
#456=EDGE_LOOP('',(#1799,#1800,#1801,#1802));
#457=EDGE_LOOP('',(#1803,#1804,#1805,#1806));
#458=EDGE_LOOP('',(#1807,#1808,#1809,#1810));
#459=EDGE_LOOP('',(#1811,#1812,#1813,#1814));
#460=EDGE_LOOP('',(#1815,#1816,#1817,#1818));
#461=EDGE_LOOP('',(#1819,#1820,#1821,#1822,#1823,#1824,#1825,#1826,#1827,
#1828,#1829,#1830,#1831,#1832,#1833,#1834,#1835,#1836));
#462=EDGE_LOOP('',(#1837));
#463=EDGE_LOOP('',(#1838));
#464=EDGE_LOOP('',(#1839));
#465=EDGE_LOOP('',(#1840));
#466=EDGE_LOOP('',(#1841,#1842,#1843,#1844));
#467=EDGE_LOOP('',(#1845,#1846,#1847,#1848));
#468=EDGE_LOOP('',(#1849,#1850,#1851,#1852,#1853,#1854));
#469=EDGE_LOOP('',(#1855,#1856,#1857,#1858));
#470=EDGE_LOOP('',(#1859));
#471=EDGE_LOOP('',(#1860));
#472=EDGE_LOOP('',(#1861));
#473=EDGE_LOOP('',(#1862));
#474=EDGE_LOOP('',(#1863,#1864,#1865,#1866,#1867,#1868));
#475=EDGE_LOOP('',(#1869));
#476=EDGE_LOOP('',(#1870,#1871,#1872,#1873,#1874,#1875));
#477=EDGE_LOOP('',(#1876));
#478=EDGE_LOOP('',(#1877,#1878,#1879,#1880));
#479=EDGE_LOOP('',(#1881,#1882,#1883,#1884));
#480=EDGE_LOOP('',(#1885,#1886,#1887,#1888));
#481=EDGE_LOOP('',(#1889,#1890,#1891,#1892));
#482=EDGE_LOOP('',(#1893,#1894,#1895,#1896));
#483=EDGE_LOOP('',(#1897,#1898,#1899,#1900));
#484=EDGE_LOOP('',(#1901,#1902,#1903,#1904));
#485=EDGE_LOOP('',(#1905));
#486=EDGE_LOOP('',(#1906));
#487=EDGE_LOOP('',(#1907,#1908,#1909,#1910));
#488=EDGE_LOOP('',(#1911,#1912,#1913,#1914));
#489=EDGE_LOOP('',(#1915,#1916,#1917,#1918));
#490=EDGE_LOOP('',(#1919));
#491=EDGE_LOOP('',(#1920));
#492=EDGE_LOOP('',(#1921,#1922,#1923,#1924));
#493=EDGE_LOOP('',(#1925,#1926,#1927));
#494=EDGE_LOOP('',(#1928,#1929,#1930,#1931));
#495=EDGE_LOOP('',(#1932,#1933,#1934,#1935));
#496=EDGE_LOOP('',(#1936));
#497=EDGE_LOOP('',(#1937));
#498=EDGE_LOOP('',(#1938,#1939,#1940,#1941));
#499=EDGE_LOOP('',(#1942));
#500=EDGE_LOOP('',(#1943,#1944,#1945,#1946));
#501=EDGE_LOOP('',(#1947));
#502=EDGE_LOOP('',(#1948));
#503=EDGE_LOOP('',(#1949,#1950,#1951,#1952));
#504=EDGE_LOOP('',(#1953));
#505=EDGE_LOOP('',(#1954,#1955,#1956,#1957));
#506=EDGE_LOOP('',(#1958));
#507=EDGE_LOOP('',(#1959,#1960,#1961,#1962));
#508=EDGE_LOOP('',(#1963));
#509=EDGE_LOOP('',(#1964));
#510=EDGE_LOOP('',(#1965,#1966,#1967,#1968));
#511=EDGE_LOOP('',(#1969,#1970,#1971,#1972));
#512=EDGE_LOOP('',(#1973,#1974,#1975,#1976));
#513=EDGE_LOOP('',(#1977,#1978,#1979,#1980));
#514=EDGE_LOOP('',(#1981,#1982,#1983,#1984));
#515=EDGE_LOOP('',(#1985,#1986,#1987,#1988,#1989));
#516=EDGE_LOOP('',(#1990,#1991,#1992,#1993,#1994));
#517=EDGE_LOOP('',(#1995,#1996,#1997,#1998));
#518=EDGE_LOOP('',(#1999,#2000,#2001,#2002));
#519=EDGE_LOOP('',(#2003));
#520=EDGE_LOOP('',(#2004,#2005,#2006,#2007,#2008,#2009,#2010,#2011,#2012));
#521=EDGE_LOOP('',(#2013,#2014,#2015,#2016));
#522=EDGE_LOOP('',(#2017,#2018,#2019,#2020));
#523=EDGE_LOOP('',(#2021,#2022,#2023,#2024));
#524=EDGE_LOOP('',(#2025,#2026,#2027,#2028));
#525=EDGE_LOOP('',(#2029,#2030,#2031,#2032));
#526=EDGE_LOOP('',(#2033,#2034,#2035,#2036));
#527=EDGE_LOOP('',(#2037));
#528=EDGE_LOOP('',(#2038,#2039,#2040,#2041,#2042,#2043));
#529=EDGE_LOOP('',(#2044));
#530=ELLIPSE('',#2313,0.565685424949238,0.4);
#531=ELLIPSE('',#2314,0.565685424949238,0.4);
#532=ELLIPSE('',#2336,0.565685424949238,0.4);
#533=ELLIPSE('',#2337,0.565685424949238,0.4);
#534=CIRCLE('',#2312,0.4);
#535=CIRCLE('',#2315,0.4);
#536=CIRCLE('',#2317,0.25);
#537=CIRCLE('',#2318,0.25);
#538=CIRCLE('',#2321,0.25);
#539=CIRCLE('',#2322,0.25);
#540=CIRCLE('',#2325,0.25);
#541=CIRCLE('',#2326,0.25);
#542=CIRCLE('',#2329,0.25);
#543=CIRCLE('',#2330,0.25);
#544=CIRCLE('',#2333,0.4);
#545=CIRCLE('',#2335,0.4);
#546=CIRCLE('',#2338,0.4);
#547=CIRCLE('',#2341,0.93);
#548=CIRCLE('',#2342,0.93);
#549=CIRCLE('',#2345,0.49);
#550=CIRCLE('',#2346,0.49);
#551=CIRCLE('',#2348,0.25);
#552=CIRCLE('',#2350,0.25);
#553=CIRCLE('',#2352,0.25);
#554=CIRCLE('',#2354,0.25);
#555=CIRCLE('',#2356,0.4);
#556=CIRCLE('',#2357,0.4);
#557=CIRCLE('',#2360,0.2);
#558=CIRCLE('',#2361,0.2);
#559=CIRCLE('',#2363,0.2);
#560=CIRCLE('',#2366,0.79);
#561=CIRCLE('',#2368,0.79);
#562=CIRCLE('',#2370,0.93);
#563=CIRCLE('',#2371,0.93);
#564=CIRCLE('',#2381,0.199999999999999);
#565=CIRCLE('',#2382,0.199999999999999);
#566=CIRCLE('',#2385,0.685);
#567=CIRCLE('',#2386,0.685);
#568=CIRCLE('',#2389,0.0250000000000004);
#569=CIRCLE('',#2391,0.93);
#570=CIRCLE('',#2392,0.93);
#571=CIRCLE('',#2402,1.7);
#572=CIRCLE('',#2404,1.7);
#573=CIRCLE('',#2406,0.55);
#574=CIRCLE('',#2407,0.55);
#575=CIRCLE('',#2408,0.55);
#576=CIRCLE('',#2409,0.55);
#577=CIRCLE('',#2410,0.55);
#578=CIRCLE('',#2412,0.33);
#579=CIRCLE('',#2413,0.33);
#580=CIRCLE('',#2414,0.33);
#581=CIRCLE('',#2416,0.33);
#582=CIRCLE('',#2417,0.33);
#583=CIRCLE('',#2418,0.33);
#584=CIRCLE('',#2420,0.55);
#585=CIRCLE('',#2421,0.55);
#586=CIRCLE('',#2422,0.55);
#587=CIRCLE('',#2423,0.55);
#588=CIRCLE('',#2426,0.55);
#589=CIRCLE('',#2427,0.55);
#590=CIRCLE('',#2428,0.55);
#591=CIRCLE('',#2429,0.33);
#592=CIRCLE('',#2430,0.33);
#593=CIRCLE('',#2431,0.33);
#594=CIRCLE('',#2432,0.33);
#595=CIRCLE('',#2434,0.33);
#596=CIRCLE('',#2436,0.55);
#597=CIRCLE('',#2437,0.55);
#598=CIRCLE('',#2438,0.55);
#599=CIRCLE('',#2439,0.33);
#600=CIRCLE('',#2440,0.33);
#601=CIRCLE('',#2442,0.55);
#602=CIRCLE('',#2445,0.33);
#603=CIRCLE('',#2449,0.33);
#604=CIRCLE('',#2452,0.55);
#605=CIRCLE('',#2453,0.55);
#606=CIRCLE('',#2455,0.33);
#607=CIRCLE('',#2458,0.33);
#608=CIRCLE('',#2460,0.33);
#609=CIRCLE('',#2469,1.065);
#610=CIRCLE('',#2471,1.065);
#611=CIRCLE('',#2479,1.065);
#612=CIRCLE('',#2481,0.985);
#613=CIRCLE('',#2482,0.79);
#614=CIRCLE('',#2485,1.065);
#615=CIRCLE('',#2487,0.985);
#616=CIRCLE('',#2489,0.79);
#617=CIRCLE('',#2493,0.2);
#618=CIRCLE('',#2495,0.3);
#619=CIRCLE('',#2497,0.3);
#620=CIRCLE('',#2499,0.6);
#621=CIRCLE('',#2501,0.6);
#622=CIRCLE('',#2505,0.089);
#623=CIRCLE('',#2506,0.3035);
#624=CIRCLE('',#2509,2.);
#625=CIRCLE('',#2510,0.685);
#626=CIRCLE('',#2512,2.);
#627=CIRCLE('',#2515,0.685);
#628=CIRCLE('',#2518,1.9);
#629=CIRCLE('',#2519,1.9);
#630=CIRCLE('',#2531,0.2942);
#631=CIRCLE('',#2532,0.2942);
#632=CIRCLE('',#2534,0.24);
#633=CIRCLE('',#2537,0.475);
#634=LINE('',#3238,#805);
#635=LINE('',#3250,#806);
#636=LINE('',#3257,#807);
#637=LINE('',#3264,#808);
#638=LINE('',#3271,#809);
#639=LINE('',#3277,#810);
#640=LINE('',#3280,#811);
#641=LINE('',#3283,#812);
#642=LINE('',#3305,#813);
#643=LINE('',#3310,#814);
#644=LINE('',#3314,#815);
#645=LINE('',#3315,#816);
#646=LINE('',#3320,#817);
#647=LINE('',#3327,#818);
#648=LINE('',#3338,#819);
#649=LINE('',#3341,#820);
#650=LINE('',#3354,#821);
#651=LINE('',#3358,#822);
#652=LINE('',#3375,#823);
#653=LINE('',#3391,#824);
#654=LINE('',#3397,#825);
#655=LINE('',#3402,#826);
#656=LINE('',#3408,#827);
#657=LINE('',#3410,#828);
#658=LINE('',#3412,#829);
#659=LINE('',#3413,#830);
#660=LINE('',#3416,#831);
#661=LINE('',#3418,#832);
#662=LINE('',#3419,#833);
#663=LINE('',#3422,#834);
#664=LINE('',#3424,#835);
#665=LINE('',#3425,#836);
#666=LINE('',#3427,#837);
#667=LINE('',#3428,#838);
#668=LINE('',#3436,#839);
#669=LINE('',#3443,#840);
#670=LINE('',#3467,#841);
#671=LINE('',#3494,#842);
#672=LINE('',#3499,#843);
#673=LINE('',#3505,#844);
#674=LINE('',#3507,#845);
#675=LINE('',#3509,#846);
#676=LINE('',#3510,#847);
#677=LINE('',#3513,#848);
#678=LINE('',#3515,#849);
#679=LINE('',#3516,#850);
#680=LINE('',#3519,#851);
#681=LINE('',#3521,#852);
#682=LINE('',#3522,#853);
#683=LINE('',#3524,#854);
#684=LINE('',#3525,#855);
#685=LINE('',#3532,#856);
#686=LINE('',#3536,#857);
#687=LINE('',#3537,#858);
#688=LINE('',#3561,#859);
#689=LINE('',#3578,#860);
#690=LINE('',#3582,#861);
#691=LINE('',#3600,#862);
#692=LINE('',#3625,#863);
#693=LINE('',#3629,#864);
#694=LINE('',#3633,#865);
#695=LINE('',#3641,#866);
#696=LINE('',#3648,#867);
#697=LINE('',#3654,#868);
#698=LINE('',#3658,#869);
#699=LINE('',#3663,#870);
#700=LINE('',#3667,#871);
#701=LINE('',#3669,#872);
#702=LINE('',#3670,#873);
#703=LINE('',#3673,#874);
#704=LINE('',#3675,#875);
#705=LINE('',#3676,#876);
#706=LINE('',#3678,#877);
#707=LINE('',#3684,#878);
#708=LINE('',#3686,#879);
#709=LINE('',#3688,#880);
#710=LINE('',#3701,#881);
#711=LINE('',#3708,#882);
#712=LINE('',#3710,#883);
#713=LINE('',#3712,#884);
#714=LINE('',#3715,#885);
#715=LINE('',#3717,#886);
#716=LINE('',#3719,#887);
#717=LINE('',#3720,#888);
#718=LINE('',#3726,#889);
#719=LINE('',#3728,#890);
#720=LINE('',#3731,#891);
#721=LINE('',#3735,#892);
#722=LINE('',#3737,#893);
#723=LINE('',#3739,#894);
#724=LINE('',#3743,#895);
#725=LINE('',#3745,#896);
#726=LINE('',#3747,#897);
#727=LINE('',#3749,#898);
#728=LINE('',#3755,#899);
#729=LINE('',#3757,#900);
#730=LINE('',#3760,#901);
#731=LINE('',#3764,#902);
#732=LINE('',#3769,#903);
#733=LINE('',#3771,#904);
#734=LINE('',#3773,#905);
#735=LINE('',#3774,#906);
#736=LINE('',#3777,#907);
#737=LINE('',#3779,#908);
#738=LINE('',#3780,#909);
#739=LINE('',#3782,#910);
#740=LINE('',#3784,#911);
#741=LINE('',#3785,#912);
#742=LINE('',#3788,#913);
#743=LINE('',#3789,#914);
#744=LINE('',#3791,#915);
#745=LINE('',#3797,#916);
#746=LINE('',#3799,#917);
#747=LINE('',#3801,#918);
#748=LINE('',#3803,#919);
#749=LINE('',#3805,#920);
#750=LINE('',#3806,#921);
#751=LINE('',#3812,#922);
#752=LINE('',#3814,#923);
#753=LINE('',#3816,#924);
#754=LINE('',#3818,#925);
#755=LINE('',#3820,#926);
#756=LINE('',#3821,#927);
#757=LINE('',#3825,#928);
#758=LINE('',#3826,#929);
#759=LINE('',#3828,#930);
#760=LINE('',#3830,#931);
#761=LINE('',#3832,#932);
#762=LINE('',#3834,#933);
#763=LINE('',#3838,#934);
#764=LINE('',#3846,#935);
#765=LINE('',#3850,#936);
#766=LINE('',#3854,#937);
#767=LINE('',#3859,#938);
#768=LINE('',#3865,#939);
#769=LINE('',#3869,#940);
#770=LINE('',#3873,#941);
#771=LINE('',#3880,#942);
#772=LINE('',#3895,#943);
#773=LINE('',#3901,#944);
#774=LINE('',#3907,#945);
#775=LINE('',#3914,#946);
#776=LINE('',#3916,#947);
#777=LINE('',#3918,#948);
#778=LINE('',#3919,#949);
#779=LINE('',#3922,#950);
#780=LINE('',#3924,#951);
#781=LINE('',#3925,#952);
#782=LINE('',#3928,#953);
#783=LINE('',#3930,#954);
#784=LINE('',#3931,#955);
#785=LINE('',#3934,#956);
#786=LINE('',#3936,#957);
#787=LINE('',#3937,#958);
#788=LINE('',#3939,#959);
#789=LINE('',#3940,#960);
#790=LINE('',#3948,#961);
#791=LINE('',#3953,#962);
#792=LINE('',#3959,#963);
#793=LINE('',#3985,#964);
#794=LINE('',#3987,#965);
#795=LINE('',#3988,#966);
#796=LINE('',#3991,#967);
#797=LINE('',#3992,#968);
#798=LINE('',#3995,#969);
#799=LINE('',#3996,#970);
#800=LINE('',#3999,#971);
#801=LINE('',#4000,#972);
#802=LINE('',#4003,#973);
#803=LINE('',#4004,#974);
#804=LINE('',#4006,#975);
#805=VECTOR('',#2567,0.4);
#806=VECTOR('',#2580,0.25);
#807=VECTOR('',#2589,0.25);
#808=VECTOR('',#2598,0.25);
#809=VECTOR('',#2607,0.25);
#810=VECTOR('',#2614,1.);
#811=VECTOR('',#2617,1.);
#812=VECTOR('',#2620,1.);
#813=VECTOR('',#2623,1.);
#814=VECTOR('',#2628,0.4);
#815=VECTOR('',#2633,1.);
#816=VECTOR('',#2634,1.);
#817=VECTOR('',#2639,0.93);
#818=VECTOR('',#2648,0.49);
#819=VECTOR('',#2663,0.25);
#820=VECTOR('',#2666,0.25);
#821=VECTOR('',#2685,1.);
#822=VECTOR('',#2690,1.);
#823=VECTOR('',#2691,0.2);
#824=VECTOR('',#2692,1.);
#825=VECTOR('',#2701,0.79);
#826=VECTOR('',#2706,0.93);
#827=VECTOR('',#2713,1.);
#828=VECTOR('',#2714,1.);
#829=VECTOR('',#2715,1.);
#830=VECTOR('',#2716,1.);
#831=VECTOR('',#2719,1.);
#832=VECTOR('',#2720,1.);
#833=VECTOR('',#2721,1.);
#834=VECTOR('',#2724,1.);
#835=VECTOR('',#2725,1.);
#836=VECTOR('',#2726,1.);
#837=VECTOR('',#2729,1.);
#838=VECTOR('',#2730,1.);
#839=VECTOR('',#2741,0.199999999999999);
#840=VECTOR('',#2750,0.685);
#841=VECTOR('',#2751,0.685);
#842=VECTOR('',#2760,0.0250000000000004);
#843=VECTOR('',#2765,0.93);
#844=VECTOR('',#2772,1.);
#845=VECTOR('',#2773,1.);
#846=VECTOR('',#2774,1.);
#847=VECTOR('',#2775,1.);
#848=VECTOR('',#2778,1.);
#849=VECTOR('',#2779,1.);
#850=VECTOR('',#2780,1.);
#851=VECTOR('',#2783,1.);
#852=VECTOR('',#2784,1.);
#853=VECTOR('',#2785,1.);
#854=VECTOR('',#2788,1.);
#855=VECTOR('',#2789,1.);
#856=VECTOR('',#2798,1.);
#857=VECTOR('',#2801,1.);
#858=VECTOR('',#2802,1.);
#859=VECTOR('',#2805,1.);
#860=VECTOR('',#2806,1.);
#861=VECTOR('',#2809,1.);
#862=VECTOR('',#2810,1.);
#863=VECTOR('',#2813,1.);
#864=VECTOR('',#2816,1.);
#865=VECTOR('',#2819,0.55);
#866=VECTOR('',#2830,0.33);
#867=VECTOR('',#2839,0.33);
#868=VECTOR('',#2846,1.);
#869=VECTOR('',#2849,0.55);
#870=VECTOR('',#2854,1.);
#871=VECTOR('',#2859,1.);
#872=VECTOR('',#2860,1.);
#873=VECTOR('',#2861,1.);
#874=VECTOR('',#2864,1.);
#875=VECTOR('',#2865,1.);
#876=VECTOR('',#2866,1.);
#877=VECTOR('',#2867,1.);
#878=VECTOR('',#2872,1.);
#879=VECTOR('',#2873,1.);
#880=VECTOR('',#2874,1.);
#881=VECTOR('',#2889,0.33);
#882=VECTOR('',#2896,1.);
#883=VECTOR('',#2897,1.);
#884=VECTOR('',#2898,1.);
#885=VECTOR('',#2901,1.);
#886=VECTOR('',#2902,1.);
#887=VECTOR('',#2903,1.);
#888=VECTOR('',#2904,1.);
#889=VECTOR('',#2911,1.);
#890=VECTOR('',#2912,0.55);
#891=VECTOR('',#2917,1.);
#892=VECTOR('',#2922,0.33);
#893=VECTOR('',#2925,1.);
#894=VECTOR('',#2928,1.);
#895=VECTOR('',#2933,0.33);
#896=VECTOR('',#2936,1.);
#897=VECTOR('',#2939,1.);
#898=VECTOR('',#2940,0.55);
#899=VECTOR('',#2949,0.33);
#900=VECTOR('',#2952,1.);
#901=VECTOR('',#2955,0.33);
#902=VECTOR('',#2960,0.33);
#903=VECTOR('',#2965,1.);
#904=VECTOR('',#2966,1.);
#905=VECTOR('',#2967,1.);
#906=VECTOR('',#2968,1.);
#907=VECTOR('',#2971,1.);
#908=VECTOR('',#2972,1.);
#909=VECTOR('',#2973,1.);
#910=VECTOR('',#2976,1.);
#911=VECTOR('',#2977,1.);
#912=VECTOR('',#2978,1.);
#913=VECTOR('',#2981,1.);
#914=VECTOR('',#2982,1.);
#915=VECTOR('',#2985,1.);
#916=VECTOR('',#2992,1.);
#917=VECTOR('',#2993,1.);
#918=VECTOR('',#2994,1.);
#919=VECTOR('',#2995,1.);
#920=VECTOR('',#2996,1.);
#921=VECTOR('',#2997,1.);
#922=VECTOR('',#3002,1.);
#923=VECTOR('',#3003,1.);
#924=VECTOR('',#3004,1.);
#925=VECTOR('',#3005,1.);
#926=VECTOR('',#3006,1.);
#927=VECTOR('',#3007,1.);
#928=VECTOR('',#3012,1.);
#929=VECTOR('',#3013,1.);
#930=VECTOR('',#3016,1.);
#931=VECTOR('',#3019,1.);
#932=VECTOR('',#3022,1.);
#933=VECTOR('',#3025,1.);
#934=VECTOR('',#3030,1.065);
#935=VECTOR('',#3041,1.025);
#936=VECTOR('',#3046,1.065);
#937=VECTOR('',#3051,1.025);
#938=VECTOR('',#3058,0.79);
#939=VECTOR('',#3065,0.1);
#940=VECTOR('',#3070,0.25);
#941=VECTOR('',#3075,0.3);
#942=VECTOR('',#3084,0.6);
#943=VECTOR('',#3105,2.);
#944=VECTOR('',#3114,0.685);
#945=VECTOR('',#3121,1.9);
#946=VECTOR('',#3130,1.);
#947=VECTOR('',#3131,1.);
#948=VECTOR('',#3132,1.);
#949=VECTOR('',#3133,1.);
#950=VECTOR('',#3136,1.);
#951=VECTOR('',#3137,1.);
#952=VECTOR('',#3138,1.);
#953=VECTOR('',#3141,1.);
#954=VECTOR('',#3142,1.);
#955=VECTOR('',#3143,1.);
#956=VECTOR('',#3146,1.);
#957=VECTOR('',#3147,1.);
#958=VECTOR('',#3148,1.);
#959=VECTOR('',#3151,1.);
#960=VECTOR('',#3152,1.);
#961=VECTOR('',#3163,0.3);
#962=VECTOR('',#3170,0.27);
#963=VECTOR('',#3177,0.576175134594813);
#964=VECTOR('',#3180,1.);
#965=VECTOR('',#3181,1.);
#966=VECTOR('',#3182,1.);
#967=VECTOR('',#3185,1.);
#968=VECTOR('',#3186,1.);
#969=VECTOR('',#3189,1.);
#970=VECTOR('',#3190,1.);
#971=VECTOR('',#3193,1.);
#972=VECTOR('',#3194,1.);
#973=VECTOR('',#3197,1.);
#974=VECTOR('',#3198,1.);
#975=VECTOR('',#3201,1.);
#976=VERTEX_POINT('',#3236);
#977=VERTEX_POINT('',#3237);
#978=VERTEX_POINT('',#3239);
#979=VERTEX_POINT('',#3241);
#980=VERTEX_POINT('',#3243);
#981=VERTEX_POINT('',#3247);
#982=VERTEX_POINT('',#3249);
#983=VERTEX_POINT('',#3254);
#984=VERTEX_POINT('',#3256);
#985=VERTEX_POINT('',#3261);
#986=VERTEX_POINT('',#3263);
#987=VERTEX_POINT('',#3268);
#988=VERTEX_POINT('',#3270);
#989=VERTEX_POINT('',#3275);
#990=VERTEX_POINT('',#3276);
#991=VERTEX_POINT('',#3278);
#992=VERTEX_POINT('',#3282);
#993=VERTEX_POINT('',#3284);
#994=VERTEX_POINT('',#3304);
#995=VERTEX_POINT('',#3306);
#996=VERTEX_POINT('',#3309);
#997=VERTEX_POINT('',#3313);
#998=VERTEX_POINT('',#3317);
#999=VERTEX_POINT('',#3319);
#1000=VERTEX_POINT('',#3324);
#1001=VERTEX_POINT('',#3326);
#1002=VERTEX_POINT('',#3330);
#1003=VERTEX_POINT('',#3333);
#1004=VERTEX_POINT('',#3336);
#1005=VERTEX_POINT('',#3340);
#1006=VERTEX_POINT('',#3348);
#1007=VERTEX_POINT('',#3352);
#1008=VERTEX_POINT('',#3353);
#1009=VERTEX_POINT('',#3357);
#1010=VERTEX_POINT('',#3359);
#1011=VERTEX_POINT('',#3376);
#1012=VERTEX_POINT('',#3395);
#1013=VERTEX_POINT('',#3399);
#1014=VERTEX_POINT('',#3401);
#1015=VERTEX_POINT('',#3406);
#1016=VERTEX_POINT('',#3407);
#1017=VERTEX_POINT('',#3409);
#1018=VERTEX_POINT('',#3411);
#1019=VERTEX_POINT('',#3415);
#1020=VERTEX_POINT('',#3417);
#1021=VERTEX_POINT('',#3421);
#1022=VERTEX_POINT('',#3423);
#1023=VERTEX_POINT('',#3433);
#1024=VERTEX_POINT('',#3435);
#1025=VERTEX_POINT('',#3440);
#1026=VERTEX_POINT('',#3442);
#1027=VERTEX_POINT('',#3444);
#1028=VERTEX_POINT('',#3455);
#1029=VERTEX_POINT('',#3466);
#1030=VERTEX_POINT('',#3469);
#1031=VERTEX_POINT('',#3492);
#1032=VERTEX_POINT('',#3496);
#1033=VERTEX_POINT('',#3498);
#1034=VERTEX_POINT('',#3503);
#1035=VERTEX_POINT('',#3504);
#1036=VERTEX_POINT('',#3506);
#1037=VERTEX_POINT('',#3508);
#1038=VERTEX_POINT('',#3512);
#1039=VERTEX_POINT('',#3514);
#1040=VERTEX_POINT('',#3518);
#1041=VERTEX_POINT('',#3520);
#1042=VERTEX_POINT('',#3530);
#1043=VERTEX_POINT('',#3531);
#1044=VERTEX_POINT('',#3533);
#1045=VERTEX_POINT('',#3535);
#1046=VERTEX_POINT('',#3539);
#1047=VERTEX_POINT('',#3560);
#1048=VERTEX_POINT('',#3562);
#1049=VERTEX_POINT('',#3577);
#1050=VERTEX_POINT('',#3579);
#1051=VERTEX_POINT('',#3581);
#1052=VERTEX_POINT('',#3583);
#1053=VERTEX_POINT('',#3599);
#1054=VERTEX_POINT('',#3623);
#1055=VERTEX_POINT('',#3624);
#1056=VERTEX_POINT('',#3626);
#1057=VERTEX_POINT('',#3628);
#1058=VERTEX_POINT('',#3630);
#1059=VERTEX_POINT('',#3632);
#1060=VERTEX_POINT('',#3638);
#1061=VERTEX_POINT('',#3640);
#1062=VERTEX_POINT('',#3645);
#1063=VERTEX_POINT('',#3647);
#1064=VERTEX_POINT('',#3652);
#1065=VERTEX_POINT('',#3653);
#1066=VERTEX_POINT('',#3655);
#1067=VERTEX_POINT('',#3657);
#1068=VERTEX_POINT('',#3660);
#1069=VERTEX_POINT('',#3662);
#1070=VERTEX_POINT('',#3666);
#1071=VERTEX_POINT('',#3668);
#1072=VERTEX_POINT('',#3672);
#1073=VERTEX_POINT('',#3674);
#1074=VERTEX_POINT('',#3677);
#1075=VERTEX_POINT('',#3679);
#1076=VERTEX_POINT('',#3681);
#1077=VERTEX_POINT('',#3683);
#1078=VERTEX_POINT('',#3685);
#1079=VERTEX_POINT('',#3687);
#1080=VERTEX_POINT('',#3690);
#1081=VERTEX_POINT('',#3692);
#1082=VERTEX_POINT('',#3694);
#1083=VERTEX_POINT('',#3696);
#1084=VERTEX_POINT('',#3699);
#1085=VERTEX_POINT('',#3703);
#1086=VERTEX_POINT('',#3705);
#1087=VERTEX_POINT('',#3707);
#1088=VERTEX_POINT('',#3709);
#1089=VERTEX_POINT('',#3711);
#1090=VERTEX_POINT('',#3713);
#1091=VERTEX_POINT('',#3716);
#1092=VERTEX_POINT('',#3718);
#1093=VERTEX_POINT('',#3721);
#1094=VERTEX_POINT('',#3723);
#1095=VERTEX_POINT('',#3727);
#1096=VERTEX_POINT('',#3733);
#1097=VERTEX_POINT('',#3741);
#1098=VERTEX_POINT('',#3748);
#1099=VERTEX_POINT('',#3753);
#1100=VERTEX_POINT('',#3759);
#1101=VERTEX_POINT('',#3763);
#1102=VERTEX_POINT('',#3767);
#1103=VERTEX_POINT('',#3768);
#1104=VERTEX_POINT('',#3770);
#1105=VERTEX_POINT('',#3772);
#1106=VERTEX_POINT('',#3776);
#1107=VERTEX_POINT('',#3778);
#1108=VERTEX_POINT('',#3783);
#1109=VERTEX_POINT('',#3787);
#1110=VERTEX_POINT('',#3795);
#1111=VERTEX_POINT('',#3796);
#1112=VERTEX_POINT('',#3798);
#1113=VERTEX_POINT('',#3800);
#1114=VERTEX_POINT('',#3802);
#1115=VERTEX_POINT('',#3804);
#1116=VERTEX_POINT('',#3807);
#1117=VERTEX_POINT('',#3810);
#1118=VERTEX_POINT('',#3811);
#1119=VERTEX_POINT('',#3813);
#1120=VERTEX_POINT('',#3815);
#1121=VERTEX_POINT('',#3817);
#1122=VERTEX_POINT('',#3819);
#1123=VERTEX_POINT('',#3822);
#1124=VERTEX_POINT('',#3837);
#1125=VERTEX_POINT('',#3841);
#1126=VERTEX_POINT('',#3843);
#1127=VERTEX_POINT('',#3848);
#1128=VERTEX_POINT('',#3852);
#1129=VERTEX_POINT('',#3856);
#1130=VERTEX_POINT('',#3862);
#1131=VERTEX_POINT('',#3864);
#1132=VERTEX_POINT('',#3867);
#1133=VERTEX_POINT('',#3871);
#1134=VERTEX_POINT('',#3875);
#1135=VERTEX_POINT('',#3878);
#1136=VERTEX_POINT('',#3884);
#1137=VERTEX_POINT('',#3889);
#1138=VERTEX_POINT('',#3891);
#1139=VERTEX_POINT('',#3894);
#1140=VERTEX_POINT('',#3899);
#1141=VERTEX_POINT('',#3904);
#1142=VERTEX_POINT('',#3906);
#1143=VERTEX_POINT('',#3912);
#1144=VERTEX_POINT('',#3913);
#1145=VERTEX_POINT('',#3915);
#1146=VERTEX_POINT('',#3917);
#1147=VERTEX_POINT('',#3921);
#1148=VERTEX_POINT('',#3923);
#1149=VERTEX_POINT('',#3927);
#1150=VERTEX_POINT('',#3929);
#1151=VERTEX_POINT('',#3933);
#1152=VERTEX_POINT('',#3935);
#1153=VERTEX_POINT('',#3945);
#1154=VERTEX_POINT('',#3947);
#1155=VERTEX_POINT('',#3951);
#1156=VERTEX_POINT('',#3956);
#1157=VERTEX_POINT('',#3958);
#1158=VERTEX_POINT('',#3960);
#1159=VERTEX_POINT('',#3964);
#1160=VERTEX_POINT('',#3968);
#1161=VERTEX_POINT('',#3972);
#1162=VERTEX_POINT('',#3976);
#1163=VERTEX_POINT('',#3984);
#1164=VERTEX_POINT('',#3986);
#1165=VERTEX_POINT('',#3990);
#1166=VERTEX_POINT('',#3994);
#1167=VERTEX_POINT('',#3998);
#1168=VERTEX_POINT('',#4002);
#1169=EDGE_CURVE('',#976,#977,#634,.T.);
#1170=EDGE_CURVE('',#978,#976,#534,.T.);
#1171=EDGE_CURVE('',#978,#979,#530,.T.);
#1172=EDGE_CURVE('',#979,#980,#531,.T.);
#1173=EDGE_CURVE('',#980,#977,#535,.T.);
#1174=EDGE_CURVE('',#981,#981,#536,.T.);
#1175=EDGE_CURVE('',#981,#982,#635,.T.);
#1176=EDGE_CURVE('',#982,#982,#537,.T.);
#1177=EDGE_CURVE('',#983,#983,#538,.T.);
#1178=EDGE_CURVE('',#983,#984,#636,.T.);
#1179=EDGE_CURVE('',#984,#984,#539,.T.);
#1180=EDGE_CURVE('',#985,#985,#540,.T.);
#1181=EDGE_CURVE('',#985,#986,#637,.T.);
#1182=EDGE_CURVE('',#986,#986,#541,.T.);
#1183=EDGE_CURVE('',#987,#987,#542,.T.);
#1184=EDGE_CURVE('',#987,#988,#638,.T.);
#1185=EDGE_CURVE('',#988,#988,#543,.T.);
#1186=EDGE_CURVE('',#989,#990,#639,.T.);
#1187=EDGE_CURVE('',#989,#991,#544,.T.);
#1188=EDGE_CURVE('',#990,#991,#640,.T.);
#1189=EDGE_CURVE('',#992,#978,#641,.T.);
#1190=EDGE_CURVE('',#993,#992,#545,.T.);
#1191=EDGE_CURVE('',#991,#993,#153,.T.);
#1192=EDGE_CURVE('',#994,#989,#642,.T.);
#1193=EDGE_CURVE('',#995,#994,#532,.T.);
#1194=EDGE_CURVE('',#980,#995,#533,.T.);
#1195=EDGE_CURVE('',#980,#996,#643,.T.);
#1196=EDGE_CURVE('',#996,#996,#546,.T.);
#1197=EDGE_CURVE('',#997,#992,#644,.T.);
#1198=EDGE_CURVE('',#993,#997,#645,.T.);
#1199=EDGE_CURVE('',#998,#998,#547,.T.);
#1200=EDGE_CURVE('',#998,#999,#646,.T.);
#1201=EDGE_CURVE('',#999,#999,#548,.T.);
#1202=EDGE_CURVE('',#1000,#1000,#549,.T.);
#1203=EDGE_CURVE('',#1000,#1001,#647,.T.);
#1204=EDGE_CURVE('',#1001,#1001,#550,.T.);
#1205=EDGE_CURVE('',#1002,#1002,#551,.T.);
#1206=EDGE_CURVE('',#1003,#1003,#552,.T.);
#1207=EDGE_CURVE('',#1004,#1004,#553,.T.);
#1208=EDGE_CURVE('',#1004,#1003,#648,.T.);
#1209=EDGE_CURVE('',#1002,#1005,#649,.T.);
#1210=EDGE_CURVE('',#1005,#1005,#554,.T.);
#1211=EDGE_CURVE('',#977,#980,#555,.T.);
#1212=EDGE_CURVE('',#976,#994,#556,.T.);
#1213=EDGE_CURVE('',#1006,#990,#557,.T.);
#1214=EDGE_CURVE('',#997,#1006,#558,.T.);
#1215=EDGE_CURVE('',#1007,#1008,#650,.T.);
#1216=EDGE_CURVE('',#1007,#1008,#559,.T.);
#1217=EDGE_CURVE('',#1009,#1007,#651,.T.);
#1218=EDGE_CURVE('',#1010,#1009,#154,.T.);
#1219=EDGE_CURVE('',#1010,#1006,#652,.T.);
#1220=EDGE_CURVE('',#1011,#1010,#155,.T.);
#1221=EDGE_CURVE('',#1008,#1011,#653,.T.);
#1222=EDGE_CURVE('',#1009,#1011,#560,.T.);
#1223=EDGE_CURVE('',#1012,#1012,#561,.T.);
#1224=EDGE_CURVE('',#1012,#1010,#654,.T.);
#1225=EDGE_CURVE('',#1013,#1013,#562,.T.);
#1226=EDGE_CURVE('',#1013,#1014,#655,.T.);
#1227=EDGE_CURVE('',#1014,#1014,#563,.T.);
#1228=EDGE_CURVE('',#1015,#1016,#656,.T.);
#1229=EDGE_CURVE('',#1016,#1017,#657,.T.);
#1230=EDGE_CURVE('',#1018,#1017,#658,.T.);
#1231=EDGE_CURVE('',#1015,#1018,#659,.T.);
#1232=EDGE_CURVE('',#1019,#1015,#660,.T.);
#1233=EDGE_CURVE('',#1020,#1018,#661,.T.);
#1234=EDGE_CURVE('',#1019,#1020,#662,.T.);
#1235=EDGE_CURVE('',#1021,#1019,#663,.T.);
#1236=EDGE_CURVE('',#1022,#1020,#664,.T.);
#1237=EDGE_CURVE('',#1021,#1022,#665,.T.);
#1238=EDGE_CURVE('',#1016,#1021,#666,.T.);
#1239=EDGE_CURVE('',#1017,#1022,#667,.T.);
#1240=EDGE_CURVE('',#1023,#1023,#564,.T.);
#1241=EDGE_CURVE('',#1023,#1024,#668,.T.);
#1242=EDGE_CURVE('',#1024,#1024,#565,.T.);
#1243=EDGE_CURVE('',#1025,#1025,#566,.T.);
#1244=EDGE_CURVE('',#1025,#1026,#669,.T.);
#1245=EDGE_CURVE('',#1027,#1026,#156,.T.);
#1246=EDGE_CURVE('',#1028,#1027,#157,.T.);
#1247=EDGE_CURVE('',#1028,#1029,#670,.T.);
#1248=EDGE_CURVE('',#1029,#1029,#567,.T.);
#1249=EDGE_CURVE('',#1030,#1028,#158,.T.);
#1250=EDGE_CURVE('',#1026,#1030,#159,.T.);
#1251=EDGE_CURVE('',#1031,#1031,#568,.T.);
#1252=EDGE_CURVE('',#1031,#1027,#671,.T.);
#1253=EDGE_CURVE('',#1032,#1032,#569,.T.);
#1254=EDGE_CURVE('',#1032,#1033,#672,.T.);
#1255=EDGE_CURVE('',#1033,#1033,#570,.T.);
#1256=EDGE_CURVE('',#1034,#1035,#673,.T.);
#1257=EDGE_CURVE('',#1035,#1036,#674,.T.);
#1258=EDGE_CURVE('',#1037,#1036,#675,.T.);
#1259=EDGE_CURVE('',#1034,#1037,#676,.T.);
#1260=EDGE_CURVE('',#1038,#1034,#677,.T.);
#1261=EDGE_CURVE('',#1039,#1037,#678,.T.);
#1262=EDGE_CURVE('',#1038,#1039,#679,.T.);
#1263=EDGE_CURVE('',#1040,#1038,#680,.T.);
#1264=EDGE_CURVE('',#1041,#1039,#681,.T.);
#1265=EDGE_CURVE('',#1040,#1041,#682,.T.);
#1266=EDGE_CURVE('',#1035,#1040,#683,.T.);
#1267=EDGE_CURVE('',#1036,#1041,#684,.T.);
#1268=EDGE_CURVE('',#1042,#1043,#685,.T.);
#1269=EDGE_CURVE('',#1044,#1042,#571,.T.);
#1270=EDGE_CURVE('',#1045,#1044,#686,.T.);
#1271=EDGE_CURVE('',#1043,#1045,#687,.T.);
#1272=EDGE_CURVE('',#1046,#1042,#160,.T.);
#1273=EDGE_CURVE('',#1047,#1046,#688,.T.);
#1274=EDGE_CURVE('',#1048,#1047,#161,.T.);
#1275=EDGE_CURVE('',#1049,#1048,#689,.T.);
#1276=EDGE_CURVE('',#1050,#1049,#572,.T.);
#1277=EDGE_CURVE('',#1051,#1050,#690,.T.);
#1278=EDGE_CURVE('',#1052,#1051,#162,.T.);
#1279=EDGE_CURVE('',#1053,#1052,#691,.T.);
#1280=EDGE_CURVE('',#1044,#1053,#163,.T.);
#1281=EDGE_CURVE('',#1054,#1055,#692,.T.);
#1282=EDGE_CURVE('',#1056,#1054,#573,.T.);
#1283=EDGE_CURVE('',#1057,#1056,#693,.T.);
#1284=EDGE_CURVE('',#1058,#1057,#574,.T.);
#1285=EDGE_CURVE('',#1058,#1059,#694,.T.);
#1286=EDGE_CURVE('',#1048,#1059,#575,.T.);
#1287=EDGE_CURVE('',#1059,#1047,#576,.T.);
#1288=EDGE_CURVE('',#1055,#1058,#577,.T.);
#1289=EDGE_CURVE('',#1060,#1060,#578,.T.);
#1290=EDGE_CURVE('',#1060,#1061,#695,.T.);
#1291=EDGE_CURVE('',#1046,#1061,#579,.T.);
#1292=EDGE_CURVE('',#1061,#1043,#580,.T.);
#1293=EDGE_CURVE('',#1062,#1062,#581,.T.);
#1294=EDGE_CURVE('',#1062,#1063,#696,.T.);
#1295=EDGE_CURVE('',#1045,#1063,#582,.T.);
#1296=EDGE_CURVE('',#1063,#1053,#583,.T.);
#1297=EDGE_CURVE('',#1064,#1065,#697,.T.);
#1298=EDGE_CURVE('',#1066,#1064,#584,.T.);
#1299=EDGE_CURVE('',#1066,#1067,#698,.T.);
#1300=EDGE_CURVE('',#1067,#1067,#585,.T.);
#1301=EDGE_CURVE('',#1068,#1066,#586,.T.);
#1302=EDGE_CURVE('',#1069,#1068,#699,.T.);
#1303=EDGE_CURVE('',#1065,#1069,#587,.T.);
#1304=EDGE_CURVE('',#1070,#1065,#700,.T.);
#1305=EDGE_CURVE('',#1070,#1071,#701,.T.);
#1306=EDGE_CURVE('',#1071,#1064,#702,.T.);
#1307=EDGE_CURVE('',#1069,#1072,#703,.T.);
#1308=EDGE_CURVE('',#1072,#1073,#704,.T.);
#1309=EDGE_CURVE('',#1073,#1055,#705,.T.);
#1310=EDGE_CURVE('',#1057,#1074,#706,.T.);
#1311=EDGE_CURVE('',#1074,#1075,#588,.T.);
#1312=EDGE_CURVE('',#1075,#1076,#589,.T.);
#1313=EDGE_CURVE('',#1076,#1077,#707,.T.);
#1314=EDGE_CURVE('',#1077,#1078,#708,.T.);
#1315=EDGE_CURVE('',#1078,#1079,#709,.T.);
#1316=EDGE_CURVE('',#1079,#1070,#590,.T.);
#1317=EDGE_CURVE('',#1080,#1080,#591,.T.);
#1318=EDGE_CURVE('',#1081,#1081,#592,.T.);
#1319=EDGE_CURVE('',#1082,#1082,#593,.T.);
#1320=EDGE_CURVE('',#1083,#1083,#594,.T.);
#1321=EDGE_CURVE('',#1084,#1084,#595,.T.);
#1322=EDGE_CURVE('',#1084,#1083,#710,.T.);
#1323=EDGE_CURVE('',#1071,#1085,#596,.T.);
#1324=EDGE_CURVE('',#1085,#1086,#597,.T.);
#1325=EDGE_CURVE('',#1087,#1086,#711,.T.);
#1326=EDGE_CURVE('',#1088,#1087,#712,.T.);
#1327=EDGE_CURVE('',#1089,#1088,#713,.T.);
#1328=EDGE_CURVE('',#1089,#1090,#598,.T.);
#1329=EDGE_CURVE('',#1056,#1090,#714,.T.);
#1330=EDGE_CURVE('',#1091,#1054,#715,.T.);
#1331=EDGE_CURVE('',#1092,#1091,#716,.T.);
#1332=EDGE_CURVE('',#1068,#1092,#717,.T.);
#1333=EDGE_CURVE('',#1093,#1093,#599,.T.);
#1334=EDGE_CURVE('',#1094,#1094,#600,.T.);
#1335=EDGE_CURVE('',#1086,#1079,#718,.T.);
#1336=EDGE_CURVE('',#1085,#1095,#719,.T.);
#1337=EDGE_CURVE('',#1095,#1095,#601,.T.);
#1338=EDGE_CURVE('',#1087,#1078,#720,.T.);
#1339=EDGE_CURVE('',#1096,#1096,#602,.T.);
#1340=EDGE_CURVE('',#1096,#1080,#721,.T.);
#1341=EDGE_CURVE('',#1072,#1092,#722,.T.);
#1342=EDGE_CURVE('',#1073,#1091,#723,.T.);
#1343=EDGE_CURVE('',#1097,#1097,#603,.T.);
#1344=EDGE_CURVE('',#1097,#1082,#724,.T.);
#1345=EDGE_CURVE('',#1090,#1074,#725,.T.);
#1346=EDGE_CURVE('',#1076,#1089,#726,.T.);
#1347=EDGE_CURVE('',#1075,#1098,#727,.T.);
#1348=EDGE_CURVE('',#1052,#1098,#604,.T.);
#1349=EDGE_CURVE('',#1098,#1051,#605,.T.);
#1350=EDGE_CURVE('',#1099,#1099,#606,.T.);
#1351=EDGE_CURVE('',#1099,#1081,#728,.T.);
#1352=EDGE_CURVE('',#1088,#1077,#729,.T.);
#1353=EDGE_CURVE('',#1094,#1100,#730,.T.);
#1354=EDGE_CURVE('',#1100,#1100,#607,.T.);
#1355=EDGE_CURVE('',#1093,#1101,#731,.T.);
#1356=EDGE_CURVE('',#1101,#1101,#608,.T.);
#1357=EDGE_CURVE('',#1102,#1103,#732,.T.);
#1358=EDGE_CURVE('',#1102,#1104,#733,.T.);
#1359=EDGE_CURVE('',#1104,#1105,#734,.T.);
#1360=EDGE_CURVE('',#1105,#1103,#735,.T.);
#1361=EDGE_CURVE('',#1106,#1103,#736,.T.);
#1362=EDGE_CURVE('',#1107,#1106,#737,.T.);
#1363=EDGE_CURVE('',#1107,#1102,#738,.T.);
#1364=EDGE_CURVE('',#1050,#1106,#739,.T.);
#1365=EDGE_CURVE('',#1108,#1105,#740,.T.);
#1366=EDGE_CURVE('',#1108,#1049,#741,.T.);
#1367=EDGE_CURVE('',#1104,#1109,#742,.T.);
#1368=EDGE_CURVE('',#1109,#1108,#743,.T.);
#1369=EDGE_CURVE('',#1109,#1107,#744,.T.);
#1370=EDGE_CURVE('',#1110,#1111,#745,.T.);
#1371=EDGE_CURVE('',#1111,#1112,#746,.T.);
#1372=EDGE_CURVE('',#1112,#1113,#747,.T.);
#1373=EDGE_CURVE('',#1113,#1114,#748,.T.);
#1374=EDGE_CURVE('',#1114,#1115,#749,.T.);
#1375=EDGE_CURVE('',#1115,#1110,#750,.T.);
#1376=EDGE_CURVE('',#1116,#1116,#609,.T.);
#1377=EDGE_CURVE('',#1117,#1118,#751,.T.);
#1378=EDGE_CURVE('',#1118,#1119,#752,.T.);
#1379=EDGE_CURVE('',#1119,#1120,#753,.T.);
#1380=EDGE_CURVE('',#1120,#1121,#754,.T.);
#1381=EDGE_CURVE('',#1121,#1122,#755,.T.);
#1382=EDGE_CURVE('',#1122,#1117,#756,.T.);
#1383=EDGE_CURVE('',#1123,#1123,#610,.T.);
#1384=EDGE_CURVE('',#1117,#1111,#757,.T.);
#1385=EDGE_CURVE('',#1112,#1122,#758,.T.);
#1386=EDGE_CURVE('',#1113,#1121,#759,.T.);
#1387=EDGE_CURVE('',#1114,#1120,#760,.T.);
#1388=EDGE_CURVE('',#1115,#1119,#761,.T.);
#1389=EDGE_CURVE('',#1110,#1118,#762,.T.);
#1390=EDGE_CURVE('',#1123,#1124,#763,.T.);
#1391=EDGE_CURVE('',#1124,#1124,#611,.T.);
#1392=EDGE_CURVE('',#1125,#1125,#612,.T.);
#1393=EDGE_CURVE('',#1126,#1126,#613,.T.);
#1394=EDGE_CURVE('',#1124,#1125,#764,.T.);
#1395=EDGE_CURVE('',#1127,#1127,#614,.T.);
#1396=EDGE_CURVE('',#1127,#1116,#765,.T.);
#1397=EDGE_CURVE('',#1128,#1128,#615,.T.);
#1398=EDGE_CURVE('',#1128,#1127,#766,.T.);
#1399=EDGE_CURVE('',#1129,#1129,#616,.T.);
#1400=EDGE_CURVE('',#1129,#1126,#767,.T.);
#1401=EDGE_CURVE('',#1130,#1130,#617,.T.);
#1402=EDGE_CURVE('',#1130,#1131,#768,.T.);
#1403=EDGE_CURVE('',#1132,#1132,#618,.T.);
#1404=EDGE_CURVE('',#1132,#1130,#769,.T.);
#1405=EDGE_CURVE('',#1133,#1133,#619,.T.);
#1406=EDGE_CURVE('',#1133,#1132,#770,.T.);
#1407=EDGE_CURVE('',#1134,#1134,#620,.T.);
#1408=EDGE_CURVE('',#1135,#1135,#621,.T.);
#1409=EDGE_CURVE('',#1135,#1134,#771,.T.);
#1410=EDGE_CURVE('',#1136,#1136,#622,.T.);
#1411=EDGE_CURVE('',#1136,#1136,#623,.T.);
#1412=EDGE_CURVE('',#1137,#1137,#624,.T.);
#1413=EDGE_CURVE('',#1138,#1138,#625,.T.);
#1414=EDGE_CURVE('',#1137,#1139,#772,.T.);
#1415=EDGE_CURVE('',#1139,#1139,#626,.T.);
#1416=EDGE_CURVE('',#1140,#1140,#627,.T.);
#1417=EDGE_CURVE('',#1140,#1138,#773,.T.);
#1418=EDGE_CURVE('',#1141,#1141,#628,.T.);
#1419=EDGE_CURVE('',#1141,#1142,#774,.T.);
#1420=EDGE_CURVE('',#1142,#1142,#629,.T.);
#1421=EDGE_CURVE('',#1143,#1144,#775,.T.);
#1422=EDGE_CURVE('',#1143,#1145,#776,.T.);
#1423=EDGE_CURVE('',#1146,#1145,#777,.T.);
#1424=EDGE_CURVE('',#1144,#1146,#778,.T.);
#1425=EDGE_CURVE('',#1144,#1147,#779,.T.);
#1426=EDGE_CURVE('',#1148,#1146,#780,.T.);
#1427=EDGE_CURVE('',#1147,#1148,#781,.T.);
#1428=EDGE_CURVE('',#1147,#1149,#782,.T.);
#1429=EDGE_CURVE('',#1150,#1148,#783,.T.);
#1430=EDGE_CURVE('',#1149,#1150,#784,.T.);
#1431=EDGE_CURVE('',#1149,#1151,#785,.T.);
#1432=EDGE_CURVE('',#1152,#1150,#786,.T.);
#1433=EDGE_CURVE('',#1151,#1152,#787,.T.);
#1434=EDGE_CURVE('',#1151,#1143,#788,.T.);
#1435=EDGE_CURVE('',#1145,#1152,#789,.T.);
#1436=EDGE_CURVE('',#1153,#1153,#630,.F.);
#1437=EDGE_CURVE('',#1153,#1154,#790,.T.);
#1438=EDGE_CURVE('',#1154,#1154,#631,.F.);
#1439=EDGE_CURVE('',#1155,#1155,#632,.T.);
#1440=EDGE_CURVE('',#1155,#1153,#791,.T.);
#1441=EDGE_CURVE('',#1156,#1156,#633,.T.);
#1442=EDGE_CURVE('',#1156,#1157,#792,.T.);
#1443=EDGE_CURVE('',#1158,#1157,#63,.T.);
#1444=EDGE_CURVE('',#1159,#1158,#64,.T.);
#1445=EDGE_CURVE('',#1160,#1159,#65,.T.);
#1446=EDGE_CURVE('',#1161,#1160,#66,.T.);
#1447=EDGE_CURVE('',#1162,#1161,#67,.T.);
#1448=EDGE_CURVE('',#1157,#1162,#68,.T.);
#1449=EDGE_CURVE('',#1163,#1161,#793,.T.);
#1450=EDGE_CURVE('',#1163,#1164,#794,.T.);
#1451=EDGE_CURVE('',#1164,#1162,#795,.T.);
#1452=EDGE_CURVE('',#1165,#1160,#796,.T.);
#1453=EDGE_CURVE('',#1165,#1163,#797,.T.);
#1454=EDGE_CURVE('',#1166,#1159,#798,.T.);
#1455=EDGE_CURVE('',#1166,#1165,#799,.T.);
#1456=EDGE_CURVE('',#1167,#1158,#800,.T.);
#1457=EDGE_CURVE('',#1167,#1166,#801,.T.);
#1458=EDGE_CURVE('',#1168,#1157,#802,.T.);
#1459=EDGE_CURVE('',#1168,#1167,#803,.T.);
#1460=EDGE_CURVE('',#1164,#1168,#804,.T.);
#1461=ORIENTED_EDGE('',*,*,#1169,.F.);
#1462=ORIENTED_EDGE('',*,*,#1170,.F.);
#1463=ORIENTED_EDGE('',*,*,#1171,.T.);
#1464=ORIENTED_EDGE('',*,*,#1172,.T.);
#1465=ORIENTED_EDGE('',*,*,#1173,.T.);
#1466=ORIENTED_EDGE('',*,*,#1174,.F.);
#1467=ORIENTED_EDGE('',*,*,#1175,.T.);
#1468=ORIENTED_EDGE('',*,*,#1176,.T.);
#1469=ORIENTED_EDGE('',*,*,#1175,.F.);
#1470=ORIENTED_EDGE('',*,*,#1176,.F.);
#1471=ORIENTED_EDGE('',*,*,#1177,.F.);
#1472=ORIENTED_EDGE('',*,*,#1178,.T.);
#1473=ORIENTED_EDGE('',*,*,#1179,.T.);
#1474=ORIENTED_EDGE('',*,*,#1178,.F.);
#1475=ORIENTED_EDGE('',*,*,#1179,.F.);
#1476=ORIENTED_EDGE('',*,*,#1180,.F.);
#1477=ORIENTED_EDGE('',*,*,#1181,.T.);
#1478=ORIENTED_EDGE('',*,*,#1182,.T.);
#1479=ORIENTED_EDGE('',*,*,#1181,.F.);
#1480=ORIENTED_EDGE('',*,*,#1182,.F.);
#1481=ORIENTED_EDGE('',*,*,#1183,.F.);
#1482=ORIENTED_EDGE('',*,*,#1184,.T.);
#1483=ORIENTED_EDGE('',*,*,#1185,.T.);
#1484=ORIENTED_EDGE('',*,*,#1184,.F.);
#1485=ORIENTED_EDGE('',*,*,#1185,.F.);
#1486=ORIENTED_EDGE('',*,*,#1186,.F.);
#1487=ORIENTED_EDGE('',*,*,#1187,.T.);
#1488=ORIENTED_EDGE('',*,*,#1188,.F.);
#1489=ORIENTED_EDGE('',*,*,#1189,.F.);
#1490=ORIENTED_EDGE('',*,*,#1190,.F.);
#1491=ORIENTED_EDGE('',*,*,#1191,.F.);
#1492=ORIENTED_EDGE('',*,*,#1187,.F.);
#1493=ORIENTED_EDGE('',*,*,#1192,.F.);
#1494=ORIENTED_EDGE('',*,*,#1193,.F.);
#1495=ORIENTED_EDGE('',*,*,#1194,.F.);
#1496=ORIENTED_EDGE('',*,*,#1195,.T.);
#1497=ORIENTED_EDGE('',*,*,#1196,.F.);
#1498=ORIENTED_EDGE('',*,*,#1195,.F.);
#1499=ORIENTED_EDGE('',*,*,#1172,.F.);
#1500=ORIENTED_EDGE('',*,*,#1171,.F.);
#1501=ORIENTED_EDGE('',*,*,#1197,.F.);
#1502=ORIENTED_EDGE('',*,*,#1198,.F.);
#1503=ORIENTED_EDGE('',*,*,#1190,.T.);
#1504=ORIENTED_EDGE('',*,*,#1199,.F.);
#1505=ORIENTED_EDGE('',*,*,#1200,.T.);
#1506=ORIENTED_EDGE('',*,*,#1201,.F.);
#1507=ORIENTED_EDGE('',*,*,#1200,.F.);
#1508=ORIENTED_EDGE('',*,*,#1199,.T.);
#1509=ORIENTED_EDGE('',*,*,#1196,.T.);
#1510=ORIENTED_EDGE('',*,*,#1202,.F.);
#1511=ORIENTED_EDGE('',*,*,#1203,.T.);
#1512=ORIENTED_EDGE('',*,*,#1204,.T.);
#1513=ORIENTED_EDGE('',*,*,#1203,.F.);
#1514=ORIENTED_EDGE('',*,*,#1204,.F.);
#1515=ORIENTED_EDGE('',*,*,#1205,.F.);
#1516=ORIENTED_EDGE('',*,*,#1202,.T.);
#1517=ORIENTED_EDGE('',*,*,#1206,.F.);
#1518=ORIENTED_EDGE('',*,*,#1207,.F.);
#1519=ORIENTED_EDGE('',*,*,#1208,.T.);
#1520=ORIENTED_EDGE('',*,*,#1206,.T.);
#1521=ORIENTED_EDGE('',*,*,#1208,.F.);
#1522=ORIENTED_EDGE('',*,*,#1205,.T.);
#1523=ORIENTED_EDGE('',*,*,#1209,.T.);
#1524=ORIENTED_EDGE('',*,*,#1210,.F.);
#1525=ORIENTED_EDGE('',*,*,#1209,.F.);
#1526=ORIENTED_EDGE('',*,*,#1169,.T.);
#1527=ORIENTED_EDGE('',*,*,#1211,.T.);
#1528=ORIENTED_EDGE('',*,*,#1194,.T.);
#1529=ORIENTED_EDGE('',*,*,#1193,.T.);
#1530=ORIENTED_EDGE('',*,*,#1212,.F.);
#1531=ORIENTED_EDGE('',*,*,#1173,.F.);
#1532=ORIENTED_EDGE('',*,*,#1211,.F.);
#1533=ORIENTED_EDGE('',*,*,#1207,.T.);
#1534=ORIENTED_EDGE('',*,*,#1189,.T.);
#1535=ORIENTED_EDGE('',*,*,#1170,.T.);
#1536=ORIENTED_EDGE('',*,*,#1212,.T.);
#1537=ORIENTED_EDGE('',*,*,#1192,.T.);
#1538=ORIENTED_EDGE('',*,*,#1186,.T.);
#1539=ORIENTED_EDGE('',*,*,#1213,.F.);
#1540=ORIENTED_EDGE('',*,*,#1214,.F.);
#1541=ORIENTED_EDGE('',*,*,#1197,.T.);
#1542=ORIENTED_EDGE('',*,*,#1215,.F.);
#1543=ORIENTED_EDGE('',*,*,#1216,.T.);
#1544=ORIENTED_EDGE('',*,*,#1217,.F.);
#1545=ORIENTED_EDGE('',*,*,#1218,.F.);
#1546=ORIENTED_EDGE('',*,*,#1219,.T.);
#1547=ORIENTED_EDGE('',*,*,#1213,.T.);
#1548=ORIENTED_EDGE('',*,*,#1188,.T.);
#1549=ORIENTED_EDGE('',*,*,#1191,.T.);
#1550=ORIENTED_EDGE('',*,*,#1198,.T.);
#1551=ORIENTED_EDGE('',*,*,#1214,.T.);
#1552=ORIENTED_EDGE('',*,*,#1219,.F.);
#1553=ORIENTED_EDGE('',*,*,#1220,.F.);
#1554=ORIENTED_EDGE('',*,*,#1221,.F.);
#1555=ORIENTED_EDGE('',*,*,#1216,.F.);
#1556=ORIENTED_EDGE('',*,*,#1217,.T.);
#1557=ORIENTED_EDGE('',*,*,#1215,.T.);
#1558=ORIENTED_EDGE('',*,*,#1221,.T.);
#1559=ORIENTED_EDGE('',*,*,#1222,.F.);
#1560=ORIENTED_EDGE('',*,*,#1223,.F.);
#1561=ORIENTED_EDGE('',*,*,#1224,.T.);
#1562=ORIENTED_EDGE('',*,*,#1218,.T.);
#1563=ORIENTED_EDGE('',*,*,#1222,.T.);
#1564=ORIENTED_EDGE('',*,*,#1220,.T.);
#1565=ORIENTED_EDGE('',*,*,#1224,.F.);
#1566=ORIENTED_EDGE('',*,*,#1225,.F.);
#1567=ORIENTED_EDGE('',*,*,#1226,.T.);
#1568=ORIENTED_EDGE('',*,*,#1227,.T.);
#1569=ORIENTED_EDGE('',*,*,#1226,.F.);
#1570=ORIENTED_EDGE('',*,*,#1227,.F.);
#1571=ORIENTED_EDGE('',*,*,#1223,.T.);
#1572=ORIENTED_EDGE('',*,*,#1228,.T.);
#1573=ORIENTED_EDGE('',*,*,#1229,.T.);
#1574=ORIENTED_EDGE('',*,*,#1230,.F.);
#1575=ORIENTED_EDGE('',*,*,#1231,.F.);
#1576=ORIENTED_EDGE('',*,*,#1232,.T.);
#1577=ORIENTED_EDGE('',*,*,#1231,.T.);
#1578=ORIENTED_EDGE('',*,*,#1233,.F.);
#1579=ORIENTED_EDGE('',*,*,#1234,.F.);
#1580=ORIENTED_EDGE('',*,*,#1201,.T.);
#1581=ORIENTED_EDGE('',*,*,#1235,.T.);
#1582=ORIENTED_EDGE('',*,*,#1234,.T.);
#1583=ORIENTED_EDGE('',*,*,#1236,.F.);
#1584=ORIENTED_EDGE('',*,*,#1237,.F.);
#1585=ORIENTED_EDGE('',*,*,#1238,.T.);
#1586=ORIENTED_EDGE('',*,*,#1237,.T.);
#1587=ORIENTED_EDGE('',*,*,#1239,.F.);
#1588=ORIENTED_EDGE('',*,*,#1229,.F.);
#1589=ORIENTED_EDGE('',*,*,#1225,.T.);
#1590=ORIENTED_EDGE('',*,*,#1239,.T.);
#1591=ORIENTED_EDGE('',*,*,#1236,.T.);
#1592=ORIENTED_EDGE('',*,*,#1233,.T.);
#1593=ORIENTED_EDGE('',*,*,#1230,.T.);
#1594=ORIENTED_EDGE('',*,*,#1210,.T.);
#1595=ORIENTED_EDGE('',*,*,#1238,.F.);
#1596=ORIENTED_EDGE('',*,*,#1228,.F.);
#1597=ORIENTED_EDGE('',*,*,#1232,.F.);
#1598=ORIENTED_EDGE('',*,*,#1235,.F.);
#1599=ORIENTED_EDGE('',*,*,#1174,.T.);
#1600=ORIENTED_EDGE('',*,*,#1177,.T.);
#1601=ORIENTED_EDGE('',*,*,#1180,.T.);
#1602=ORIENTED_EDGE('',*,*,#1183,.T.);
#1603=ORIENTED_EDGE('',*,*,#1240,.F.);
#1604=ORIENTED_EDGE('',*,*,#1241,.T.);
#1605=ORIENTED_EDGE('',*,*,#1242,.T.);
#1606=ORIENTED_EDGE('',*,*,#1241,.F.);
#1607=ORIENTED_EDGE('',*,*,#1242,.F.);
#1608=ORIENTED_EDGE('',*,*,#1243,.F.);
#1609=ORIENTED_EDGE('',*,*,#1244,.T.);
#1610=ORIENTED_EDGE('',*,*,#1245,.F.);
#1611=ORIENTED_EDGE('',*,*,#1246,.F.);
#1612=ORIENTED_EDGE('',*,*,#1247,.T.);
#1613=ORIENTED_EDGE('',*,*,#1248,.T.);
#1614=ORIENTED_EDGE('',*,*,#1247,.F.);
#1615=ORIENTED_EDGE('',*,*,#1249,.F.);
#1616=ORIENTED_EDGE('',*,*,#1250,.F.);
#1617=ORIENTED_EDGE('',*,*,#1244,.F.);
#1618=ORIENTED_EDGE('',*,*,#1248,.F.);
#1619=ORIENTED_EDGE('',*,*,#1240,.T.);
#1620=ORIENTED_EDGE('',*,*,#1251,.F.);
#1621=ORIENTED_EDGE('',*,*,#1252,.T.);
#1622=ORIENTED_EDGE('',*,*,#1245,.T.);
#1623=ORIENTED_EDGE('',*,*,#1250,.T.);
#1624=ORIENTED_EDGE('',*,*,#1249,.T.);
#1625=ORIENTED_EDGE('',*,*,#1246,.T.);
#1626=ORIENTED_EDGE('',*,*,#1252,.F.);
#1627=ORIENTED_EDGE('',*,*,#1253,.F.);
#1628=ORIENTED_EDGE('',*,*,#1254,.T.);
#1629=ORIENTED_EDGE('',*,*,#1255,.T.);
#1630=ORIENTED_EDGE('',*,*,#1254,.F.);
#1631=ORIENTED_EDGE('',*,*,#1255,.F.);
#1632=ORIENTED_EDGE('',*,*,#1251,.T.);
#1633=ORIENTED_EDGE('',*,*,#1256,.T.);
#1634=ORIENTED_EDGE('',*,*,#1257,.T.);
#1635=ORIENTED_EDGE('',*,*,#1258,.F.);
#1636=ORIENTED_EDGE('',*,*,#1259,.F.);
#1637=ORIENTED_EDGE('',*,*,#1260,.T.);
#1638=ORIENTED_EDGE('',*,*,#1259,.T.);
#1639=ORIENTED_EDGE('',*,*,#1261,.F.);
#1640=ORIENTED_EDGE('',*,*,#1262,.F.);
#1641=ORIENTED_EDGE('',*,*,#1263,.T.);
#1642=ORIENTED_EDGE('',*,*,#1262,.T.);
#1643=ORIENTED_EDGE('',*,*,#1264,.F.);
#1644=ORIENTED_EDGE('',*,*,#1265,.F.);
#1645=ORIENTED_EDGE('',*,*,#1243,.T.);
#1646=ORIENTED_EDGE('',*,*,#1266,.T.);
#1647=ORIENTED_EDGE('',*,*,#1265,.T.);
#1648=ORIENTED_EDGE('',*,*,#1267,.F.);
#1649=ORIENTED_EDGE('',*,*,#1257,.F.);
#1650=ORIENTED_EDGE('',*,*,#1253,.T.);
#1651=ORIENTED_EDGE('',*,*,#1267,.T.);
#1652=ORIENTED_EDGE('',*,*,#1264,.T.);
#1653=ORIENTED_EDGE('',*,*,#1261,.T.);
#1654=ORIENTED_EDGE('',*,*,#1258,.T.);
#1655=ORIENTED_EDGE('',*,*,#1266,.F.);
#1656=ORIENTED_EDGE('',*,*,#1256,.F.);
#1657=ORIENTED_EDGE('',*,*,#1260,.F.);
#1658=ORIENTED_EDGE('',*,*,#1263,.F.);
#1659=ORIENTED_EDGE('',*,*,#1268,.F.);
#1660=ORIENTED_EDGE('',*,*,#1269,.F.);
#1661=ORIENTED_EDGE('',*,*,#1270,.F.);
#1662=ORIENTED_EDGE('',*,*,#1271,.F.);
#1663=ORIENTED_EDGE('',*,*,#1272,.F.);
#1664=ORIENTED_EDGE('',*,*,#1273,.F.);
#1665=ORIENTED_EDGE('',*,*,#1274,.F.);
#1666=ORIENTED_EDGE('',*,*,#1275,.F.);
#1667=ORIENTED_EDGE('',*,*,#1276,.F.);
#1668=ORIENTED_EDGE('',*,*,#1277,.F.);
#1669=ORIENTED_EDGE('',*,*,#1278,.F.);
#1670=ORIENTED_EDGE('',*,*,#1279,.F.);
#1671=ORIENTED_EDGE('',*,*,#1280,.F.);
#1672=ORIENTED_EDGE('',*,*,#1269,.T.);
#1673=ORIENTED_EDGE('',*,*,#1281,.F.);
#1674=ORIENTED_EDGE('',*,*,#1282,.F.);
#1675=ORIENTED_EDGE('',*,*,#1283,.F.);
#1676=ORIENTED_EDGE('',*,*,#1284,.F.);
#1677=ORIENTED_EDGE('',*,*,#1285,.T.);
#1678=ORIENTED_EDGE('',*,*,#1286,.F.);
#1679=ORIENTED_EDGE('',*,*,#1274,.T.);
#1680=ORIENTED_EDGE('',*,*,#1287,.F.);
#1681=ORIENTED_EDGE('',*,*,#1285,.F.);
#1682=ORIENTED_EDGE('',*,*,#1288,.F.);
#1683=ORIENTED_EDGE('',*,*,#1289,.F.);
#1684=ORIENTED_EDGE('',*,*,#1290,.T.);
#1685=ORIENTED_EDGE('',*,*,#1291,.F.);
#1686=ORIENTED_EDGE('',*,*,#1272,.T.);
#1687=ORIENTED_EDGE('',*,*,#1268,.T.);
#1688=ORIENTED_EDGE('',*,*,#1292,.F.);
#1689=ORIENTED_EDGE('',*,*,#1290,.F.);
#1690=ORIENTED_EDGE('',*,*,#1293,.F.);
#1691=ORIENTED_EDGE('',*,*,#1294,.T.);
#1692=ORIENTED_EDGE('',*,*,#1295,.F.);
#1693=ORIENTED_EDGE('',*,*,#1270,.T.);
#1694=ORIENTED_EDGE('',*,*,#1280,.T.);
#1695=ORIENTED_EDGE('',*,*,#1296,.F.);
#1696=ORIENTED_EDGE('',*,*,#1294,.F.);
#1697=ORIENTED_EDGE('',*,*,#1297,.F.);
#1698=ORIENTED_EDGE('',*,*,#1298,.F.);
#1699=ORIENTED_EDGE('',*,*,#1299,.T.);
#1700=ORIENTED_EDGE('',*,*,#1300,.F.);
#1701=ORIENTED_EDGE('',*,*,#1299,.F.);
#1702=ORIENTED_EDGE('',*,*,#1301,.F.);
#1703=ORIENTED_EDGE('',*,*,#1302,.F.);
#1704=ORIENTED_EDGE('',*,*,#1303,.F.);
#1705=ORIENTED_EDGE('',*,*,#1297,.T.);
#1706=ORIENTED_EDGE('',*,*,#1304,.F.);
#1707=ORIENTED_EDGE('',*,*,#1305,.T.);
#1708=ORIENTED_EDGE('',*,*,#1306,.T.);
#1709=ORIENTED_EDGE('',*,*,#1307,.T.);
#1710=ORIENTED_EDGE('',*,*,#1308,.T.);
#1711=ORIENTED_EDGE('',*,*,#1309,.T.);
#1712=ORIENTED_EDGE('',*,*,#1288,.T.);
#1713=ORIENTED_EDGE('',*,*,#1284,.T.);
#1714=ORIENTED_EDGE('',*,*,#1310,.T.);
#1715=ORIENTED_EDGE('',*,*,#1311,.T.);
#1716=ORIENTED_EDGE('',*,*,#1312,.T.);
#1717=ORIENTED_EDGE('',*,*,#1313,.T.);
#1718=ORIENTED_EDGE('',*,*,#1314,.T.);
#1719=ORIENTED_EDGE('',*,*,#1315,.T.);
#1720=ORIENTED_EDGE('',*,*,#1316,.T.);
#1721=ORIENTED_EDGE('',*,*,#1304,.T.);
#1722=ORIENTED_EDGE('',*,*,#1303,.T.);
#1723=ORIENTED_EDGE('',*,*,#1317,.F.);
#1724=ORIENTED_EDGE('',*,*,#1318,.F.);
#1725=ORIENTED_EDGE('',*,*,#1319,.T.);
#1726=ORIENTED_EDGE('',*,*,#1320,.T.);
#1727=ORIENTED_EDGE('',*,*,#1321,.F.);
#1728=ORIENTED_EDGE('',*,*,#1322,.T.);
#1729=ORIENTED_EDGE('',*,*,#1320,.F.);
#1730=ORIENTED_EDGE('',*,*,#1322,.F.);
#1731=ORIENTED_EDGE('',*,*,#1301,.T.);
#1732=ORIENTED_EDGE('',*,*,#1298,.T.);
#1733=ORIENTED_EDGE('',*,*,#1306,.F.);
#1734=ORIENTED_EDGE('',*,*,#1323,.T.);
#1735=ORIENTED_EDGE('',*,*,#1324,.T.);
#1736=ORIENTED_EDGE('',*,*,#1325,.F.);
#1737=ORIENTED_EDGE('',*,*,#1326,.F.);
#1738=ORIENTED_EDGE('',*,*,#1327,.F.);
#1739=ORIENTED_EDGE('',*,*,#1328,.T.);
#1740=ORIENTED_EDGE('',*,*,#1329,.F.);
#1741=ORIENTED_EDGE('',*,*,#1282,.T.);
#1742=ORIENTED_EDGE('',*,*,#1330,.F.);
#1743=ORIENTED_EDGE('',*,*,#1331,.F.);
#1744=ORIENTED_EDGE('',*,*,#1332,.F.);
#1745=ORIENTED_EDGE('',*,*,#1293,.T.);
#1746=ORIENTED_EDGE('',*,*,#1289,.T.);
#1747=ORIENTED_EDGE('',*,*,#1333,.T.);
#1748=ORIENTED_EDGE('',*,*,#1334,.T.);
#1749=ORIENTED_EDGE('',*,*,#1335,.F.);
#1750=ORIENTED_EDGE('',*,*,#1324,.F.);
#1751=ORIENTED_EDGE('',*,*,#1336,.T.);
#1752=ORIENTED_EDGE('',*,*,#1337,.F.);
#1753=ORIENTED_EDGE('',*,*,#1336,.F.);
#1754=ORIENTED_EDGE('',*,*,#1323,.F.);
#1755=ORIENTED_EDGE('',*,*,#1305,.F.);
#1756=ORIENTED_EDGE('',*,*,#1316,.F.);
#1757=ORIENTED_EDGE('',*,*,#1335,.T.);
#1758=ORIENTED_EDGE('',*,*,#1315,.F.);
#1759=ORIENTED_EDGE('',*,*,#1338,.F.);
#1760=ORIENTED_EDGE('',*,*,#1325,.T.);
#1761=ORIENTED_EDGE('',*,*,#1339,.F.);
#1762=ORIENTED_EDGE('',*,*,#1340,.T.);
#1763=ORIENTED_EDGE('',*,*,#1317,.T.);
#1764=ORIENTED_EDGE('',*,*,#1340,.F.);
#1765=ORIENTED_EDGE('',*,*,#1302,.T.);
#1766=ORIENTED_EDGE('',*,*,#1332,.T.);
#1767=ORIENTED_EDGE('',*,*,#1341,.F.);
#1768=ORIENTED_EDGE('',*,*,#1307,.F.);
#1769=ORIENTED_EDGE('',*,*,#1281,.T.);
#1770=ORIENTED_EDGE('',*,*,#1309,.F.);
#1771=ORIENTED_EDGE('',*,*,#1342,.T.);
#1772=ORIENTED_EDGE('',*,*,#1330,.T.);
#1773=ORIENTED_EDGE('',*,*,#1343,.F.);
#1774=ORIENTED_EDGE('',*,*,#1344,.T.);
#1775=ORIENTED_EDGE('',*,*,#1319,.F.);
#1776=ORIENTED_EDGE('',*,*,#1344,.F.);
#1777=ORIENTED_EDGE('',*,*,#1283,.T.);
#1778=ORIENTED_EDGE('',*,*,#1329,.T.);
#1779=ORIENTED_EDGE('',*,*,#1345,.T.);
#1780=ORIENTED_EDGE('',*,*,#1310,.F.);
#1781=ORIENTED_EDGE('',*,*,#1345,.F.);
#1782=ORIENTED_EDGE('',*,*,#1328,.F.);
#1783=ORIENTED_EDGE('',*,*,#1346,.F.);
#1784=ORIENTED_EDGE('',*,*,#1312,.F.);
#1785=ORIENTED_EDGE('',*,*,#1347,.T.);
#1786=ORIENTED_EDGE('',*,*,#1348,.F.);
#1787=ORIENTED_EDGE('',*,*,#1278,.T.);
#1788=ORIENTED_EDGE('',*,*,#1349,.F.);
#1789=ORIENTED_EDGE('',*,*,#1347,.F.);
#1790=ORIENTED_EDGE('',*,*,#1311,.F.);
#1791=ORIENTED_EDGE('',*,*,#1350,.F.);
#1792=ORIENTED_EDGE('',*,*,#1351,.T.);
#1793=ORIENTED_EDGE('',*,*,#1318,.T.);
#1794=ORIENTED_EDGE('',*,*,#1351,.F.);
#1795=ORIENTED_EDGE('',*,*,#1346,.T.);
#1796=ORIENTED_EDGE('',*,*,#1327,.T.);
#1797=ORIENTED_EDGE('',*,*,#1352,.T.);
#1798=ORIENTED_EDGE('',*,*,#1313,.F.);
#1799=ORIENTED_EDGE('',*,*,#1334,.F.);
#1800=ORIENTED_EDGE('',*,*,#1353,.T.);
#1801=ORIENTED_EDGE('',*,*,#1354,.F.);
#1802=ORIENTED_EDGE('',*,*,#1353,.F.);
#1803=ORIENTED_EDGE('',*,*,#1333,.F.);
#1804=ORIENTED_EDGE('',*,*,#1355,.T.);
#1805=ORIENTED_EDGE('',*,*,#1356,.F.);
#1806=ORIENTED_EDGE('',*,*,#1355,.F.);
#1807=ORIENTED_EDGE('',*,*,#1357,.F.);
#1808=ORIENTED_EDGE('',*,*,#1358,.T.);
#1809=ORIENTED_EDGE('',*,*,#1359,.T.);
#1810=ORIENTED_EDGE('',*,*,#1360,.T.);
#1811=ORIENTED_EDGE('',*,*,#1361,.F.);
#1812=ORIENTED_EDGE('',*,*,#1362,.F.);
#1813=ORIENTED_EDGE('',*,*,#1363,.T.);
#1814=ORIENTED_EDGE('',*,*,#1357,.T.);
#1815=ORIENTED_EDGE('',*,*,#1338,.T.);
#1816=ORIENTED_EDGE('',*,*,#1314,.F.);
#1817=ORIENTED_EDGE('',*,*,#1352,.F.);
#1818=ORIENTED_EDGE('',*,*,#1326,.T.);
#1819=ORIENTED_EDGE('',*,*,#1275,.T.);
#1820=ORIENTED_EDGE('',*,*,#1286,.T.);
#1821=ORIENTED_EDGE('',*,*,#1287,.T.);
#1822=ORIENTED_EDGE('',*,*,#1273,.T.);
#1823=ORIENTED_EDGE('',*,*,#1291,.T.);
#1824=ORIENTED_EDGE('',*,*,#1292,.T.);
#1825=ORIENTED_EDGE('',*,*,#1271,.T.);
#1826=ORIENTED_EDGE('',*,*,#1295,.T.);
#1827=ORIENTED_EDGE('',*,*,#1296,.T.);
#1828=ORIENTED_EDGE('',*,*,#1279,.T.);
#1829=ORIENTED_EDGE('',*,*,#1348,.T.);
#1830=ORIENTED_EDGE('',*,*,#1349,.T.);
#1831=ORIENTED_EDGE('',*,*,#1277,.T.);
#1832=ORIENTED_EDGE('',*,*,#1364,.T.);
#1833=ORIENTED_EDGE('',*,*,#1361,.T.);
#1834=ORIENTED_EDGE('',*,*,#1360,.F.);
#1835=ORIENTED_EDGE('',*,*,#1365,.F.);
#1836=ORIENTED_EDGE('',*,*,#1366,.T.);
#1837=ORIENTED_EDGE('',*,*,#1356,.T.);
#1838=ORIENTED_EDGE('',*,*,#1354,.T.);
#1839=ORIENTED_EDGE('',*,*,#1337,.T.);
#1840=ORIENTED_EDGE('',*,*,#1300,.T.);
#1841=ORIENTED_EDGE('',*,*,#1365,.T.);
#1842=ORIENTED_EDGE('',*,*,#1359,.F.);
#1843=ORIENTED_EDGE('',*,*,#1367,.T.);
#1844=ORIENTED_EDGE('',*,*,#1368,.T.);
#1845=ORIENTED_EDGE('',*,*,#1331,.T.);
#1846=ORIENTED_EDGE('',*,*,#1342,.F.);
#1847=ORIENTED_EDGE('',*,*,#1308,.F.);
#1848=ORIENTED_EDGE('',*,*,#1341,.T.);
#1849=ORIENTED_EDGE('',*,*,#1276,.T.);
#1850=ORIENTED_EDGE('',*,*,#1366,.F.);
#1851=ORIENTED_EDGE('',*,*,#1368,.F.);
#1852=ORIENTED_EDGE('',*,*,#1369,.T.);
#1853=ORIENTED_EDGE('',*,*,#1362,.T.);
#1854=ORIENTED_EDGE('',*,*,#1364,.F.);
#1855=ORIENTED_EDGE('',*,*,#1369,.F.);
#1856=ORIENTED_EDGE('',*,*,#1367,.F.);
#1857=ORIENTED_EDGE('',*,*,#1358,.F.);
#1858=ORIENTED_EDGE('',*,*,#1363,.F.);
#1859=ORIENTED_EDGE('',*,*,#1321,.T.);
#1860=ORIENTED_EDGE('',*,*,#1339,.T.);
#1861=ORIENTED_EDGE('',*,*,#1343,.T.);
#1862=ORIENTED_EDGE('',*,*,#1350,.T.);
#1863=ORIENTED_EDGE('',*,*,#1370,.T.);
#1864=ORIENTED_EDGE('',*,*,#1371,.T.);
#1865=ORIENTED_EDGE('',*,*,#1372,.T.);
#1866=ORIENTED_EDGE('',*,*,#1373,.T.);
#1867=ORIENTED_EDGE('',*,*,#1374,.T.);
#1868=ORIENTED_EDGE('',*,*,#1375,.T.);
#1869=ORIENTED_EDGE('',*,*,#1376,.F.);
#1870=ORIENTED_EDGE('',*,*,#1377,.T.);
#1871=ORIENTED_EDGE('',*,*,#1378,.T.);
#1872=ORIENTED_EDGE('',*,*,#1379,.T.);
#1873=ORIENTED_EDGE('',*,*,#1380,.T.);
#1874=ORIENTED_EDGE('',*,*,#1381,.T.);
#1875=ORIENTED_EDGE('',*,*,#1382,.T.);
#1876=ORIENTED_EDGE('',*,*,#1383,.F.);
#1877=ORIENTED_EDGE('',*,*,#1384,.F.);
#1878=ORIENTED_EDGE('',*,*,#1382,.F.);
#1879=ORIENTED_EDGE('',*,*,#1385,.F.);
#1880=ORIENTED_EDGE('',*,*,#1371,.F.);
#1881=ORIENTED_EDGE('',*,*,#1385,.T.);
#1882=ORIENTED_EDGE('',*,*,#1381,.F.);
#1883=ORIENTED_EDGE('',*,*,#1386,.F.);
#1884=ORIENTED_EDGE('',*,*,#1372,.F.);
#1885=ORIENTED_EDGE('',*,*,#1386,.T.);
#1886=ORIENTED_EDGE('',*,*,#1380,.F.);
#1887=ORIENTED_EDGE('',*,*,#1387,.F.);
#1888=ORIENTED_EDGE('',*,*,#1373,.F.);
#1889=ORIENTED_EDGE('',*,*,#1387,.T.);
#1890=ORIENTED_EDGE('',*,*,#1379,.F.);
#1891=ORIENTED_EDGE('',*,*,#1388,.F.);
#1892=ORIENTED_EDGE('',*,*,#1374,.F.);
#1893=ORIENTED_EDGE('',*,*,#1388,.T.);
#1894=ORIENTED_EDGE('',*,*,#1378,.F.);
#1895=ORIENTED_EDGE('',*,*,#1389,.F.);
#1896=ORIENTED_EDGE('',*,*,#1375,.F.);
#1897=ORIENTED_EDGE('',*,*,#1389,.T.);
#1898=ORIENTED_EDGE('',*,*,#1377,.F.);
#1899=ORIENTED_EDGE('',*,*,#1384,.T.);
#1900=ORIENTED_EDGE('',*,*,#1370,.F.);
#1901=ORIENTED_EDGE('',*,*,#1383,.T.);
#1902=ORIENTED_EDGE('',*,*,#1390,.T.);
#1903=ORIENTED_EDGE('',*,*,#1391,.T.);
#1904=ORIENTED_EDGE('',*,*,#1390,.F.);
#1905=ORIENTED_EDGE('',*,*,#1392,.F.);
#1906=ORIENTED_EDGE('',*,*,#1393,.T.);
#1907=ORIENTED_EDGE('',*,*,#1391,.F.);
#1908=ORIENTED_EDGE('',*,*,#1394,.T.);
#1909=ORIENTED_EDGE('',*,*,#1392,.T.);
#1910=ORIENTED_EDGE('',*,*,#1394,.F.);
#1911=ORIENTED_EDGE('',*,*,#1395,.F.);
#1912=ORIENTED_EDGE('',*,*,#1396,.T.);
#1913=ORIENTED_EDGE('',*,*,#1376,.T.);
#1914=ORIENTED_EDGE('',*,*,#1396,.F.);
#1915=ORIENTED_EDGE('',*,*,#1397,.F.);
#1916=ORIENTED_EDGE('',*,*,#1398,.T.);
#1917=ORIENTED_EDGE('',*,*,#1395,.T.);
#1918=ORIENTED_EDGE('',*,*,#1398,.F.);
#1919=ORIENTED_EDGE('',*,*,#1397,.T.);
#1920=ORIENTED_EDGE('',*,*,#1399,.F.);
#1921=ORIENTED_EDGE('',*,*,#1399,.T.);
#1922=ORIENTED_EDGE('',*,*,#1400,.T.);
#1923=ORIENTED_EDGE('',*,*,#1393,.F.);
#1924=ORIENTED_EDGE('',*,*,#1400,.F.);
#1925=ORIENTED_EDGE('',*,*,#1401,.F.);
#1926=ORIENTED_EDGE('',*,*,#1402,.T.);
#1927=ORIENTED_EDGE('',*,*,#1402,.F.);
#1928=ORIENTED_EDGE('',*,*,#1403,.F.);
#1929=ORIENTED_EDGE('',*,*,#1404,.T.);
#1930=ORIENTED_EDGE('',*,*,#1401,.T.);
#1931=ORIENTED_EDGE('',*,*,#1404,.F.);
#1932=ORIENTED_EDGE('',*,*,#1405,.F.);
#1933=ORIENTED_EDGE('',*,*,#1406,.T.);
#1934=ORIENTED_EDGE('',*,*,#1403,.T.);
#1935=ORIENTED_EDGE('',*,*,#1406,.F.);
#1936=ORIENTED_EDGE('',*,*,#1407,.F.);
#1937=ORIENTED_EDGE('',*,*,#1405,.T.);
#1938=ORIENTED_EDGE('',*,*,#1408,.F.);
#1939=ORIENTED_EDGE('',*,*,#1409,.T.);
#1940=ORIENTED_EDGE('',*,*,#1407,.T.);
#1941=ORIENTED_EDGE('',*,*,#1409,.F.);
#1942=ORIENTED_EDGE('',*,*,#1408,.T.);
#1943=ORIENTED_EDGE('',*,*,#1410,.F.);
#1944=ORIENTED_EDGE('',*,*,#1411,.T.);
#1945=ORIENTED_EDGE('',*,*,#1410,.T.);
#1946=ORIENTED_EDGE('',*,*,#1411,.F.);
#1947=ORIENTED_EDGE('',*,*,#1412,.T.);
#1948=ORIENTED_EDGE('',*,*,#1413,.F.);
#1949=ORIENTED_EDGE('',*,*,#1412,.F.);
#1950=ORIENTED_EDGE('',*,*,#1414,.T.);
#1951=ORIENTED_EDGE('',*,*,#1415,.T.);
#1952=ORIENTED_EDGE('',*,*,#1414,.F.);
#1953=ORIENTED_EDGE('',*,*,#1415,.F.);
#1954=ORIENTED_EDGE('',*,*,#1416,.F.);
#1955=ORIENTED_EDGE('',*,*,#1417,.T.);
#1956=ORIENTED_EDGE('',*,*,#1413,.T.);
#1957=ORIENTED_EDGE('',*,*,#1417,.F.);
#1958=ORIENTED_EDGE('',*,*,#1416,.T.);
#1959=ORIENTED_EDGE('',*,*,#1418,.F.);
#1960=ORIENTED_EDGE('',*,*,#1419,.T.);
#1961=ORIENTED_EDGE('',*,*,#1420,.T.);
#1962=ORIENTED_EDGE('',*,*,#1419,.F.);
#1963=ORIENTED_EDGE('',*,*,#1418,.T.);
#1964=ORIENTED_EDGE('',*,*,#1420,.F.);
#1965=ORIENTED_EDGE('',*,*,#1421,.F.);
#1966=ORIENTED_EDGE('',*,*,#1422,.T.);
#1967=ORIENTED_EDGE('',*,*,#1423,.F.);
#1968=ORIENTED_EDGE('',*,*,#1424,.F.);
#1969=ORIENTED_EDGE('',*,*,#1425,.F.);
#1970=ORIENTED_EDGE('',*,*,#1424,.T.);
#1971=ORIENTED_EDGE('',*,*,#1426,.F.);
#1972=ORIENTED_EDGE('',*,*,#1427,.F.);
#1973=ORIENTED_EDGE('',*,*,#1428,.F.);
#1974=ORIENTED_EDGE('',*,*,#1427,.T.);
#1975=ORIENTED_EDGE('',*,*,#1429,.F.);
#1976=ORIENTED_EDGE('',*,*,#1430,.F.);
#1977=ORIENTED_EDGE('',*,*,#1431,.F.);
#1978=ORIENTED_EDGE('',*,*,#1430,.T.);
#1979=ORIENTED_EDGE('',*,*,#1432,.F.);
#1980=ORIENTED_EDGE('',*,*,#1433,.F.);
#1981=ORIENTED_EDGE('',*,*,#1434,.F.);
#1982=ORIENTED_EDGE('',*,*,#1433,.T.);
#1983=ORIENTED_EDGE('',*,*,#1435,.F.);
#1984=ORIENTED_EDGE('',*,*,#1422,.F.);
#1985=ORIENTED_EDGE('',*,*,#1435,.T.);
#1986=ORIENTED_EDGE('',*,*,#1432,.T.);
#1987=ORIENTED_EDGE('',*,*,#1429,.T.);
#1988=ORIENTED_EDGE('',*,*,#1426,.T.);
#1989=ORIENTED_EDGE('',*,*,#1423,.T.);
#1990=ORIENTED_EDGE('',*,*,#1434,.T.);
#1991=ORIENTED_EDGE('',*,*,#1421,.T.);
#1992=ORIENTED_EDGE('',*,*,#1425,.T.);
#1993=ORIENTED_EDGE('',*,*,#1428,.T.);
#1994=ORIENTED_EDGE('',*,*,#1431,.T.);
#1995=ORIENTED_EDGE('',*,*,#1436,.F.);
#1996=ORIENTED_EDGE('',*,*,#1437,.T.);
#1997=ORIENTED_EDGE('',*,*,#1438,.F.);
#1998=ORIENTED_EDGE('',*,*,#1437,.F.);
#1999=ORIENTED_EDGE('',*,*,#1439,.F.);
#2000=ORIENTED_EDGE('',*,*,#1440,.T.);
#2001=ORIENTED_EDGE('',*,*,#1436,.T.);
#2002=ORIENTED_EDGE('',*,*,#1440,.F.);
#2003=ORIENTED_EDGE('',*,*,#1439,.T.);
#2004=ORIENTED_EDGE('',*,*,#1441,.F.);
#2005=ORIENTED_EDGE('',*,*,#1442,.T.);
#2006=ORIENTED_EDGE('',*,*,#1443,.F.);
#2007=ORIENTED_EDGE('',*,*,#1444,.F.);
#2008=ORIENTED_EDGE('',*,*,#1445,.F.);
#2009=ORIENTED_EDGE('',*,*,#1446,.F.);
#2010=ORIENTED_EDGE('',*,*,#1447,.F.);
#2011=ORIENTED_EDGE('',*,*,#1448,.F.);
#2012=ORIENTED_EDGE('',*,*,#1442,.F.);
#2013=ORIENTED_EDGE('',*,*,#1447,.T.);
#2014=ORIENTED_EDGE('',*,*,#1449,.F.);
#2015=ORIENTED_EDGE('',*,*,#1450,.T.);
#2016=ORIENTED_EDGE('',*,*,#1451,.T.);
#2017=ORIENTED_EDGE('',*,*,#1446,.T.);
#2018=ORIENTED_EDGE('',*,*,#1452,.F.);
#2019=ORIENTED_EDGE('',*,*,#1453,.T.);
#2020=ORIENTED_EDGE('',*,*,#1449,.T.);
#2021=ORIENTED_EDGE('',*,*,#1445,.T.);
#2022=ORIENTED_EDGE('',*,*,#1454,.F.);
#2023=ORIENTED_EDGE('',*,*,#1455,.T.);
#2024=ORIENTED_EDGE('',*,*,#1452,.T.);
#2025=ORIENTED_EDGE('',*,*,#1444,.T.);
#2026=ORIENTED_EDGE('',*,*,#1456,.F.);
#2027=ORIENTED_EDGE('',*,*,#1457,.T.);
#2028=ORIENTED_EDGE('',*,*,#1454,.T.);
#2029=ORIENTED_EDGE('',*,*,#1443,.T.);
#2030=ORIENTED_EDGE('',*,*,#1458,.F.);
#2031=ORIENTED_EDGE('',*,*,#1459,.T.);
#2032=ORIENTED_EDGE('',*,*,#1456,.T.);
#2033=ORIENTED_EDGE('',*,*,#1448,.T.);
#2034=ORIENTED_EDGE('',*,*,#1451,.F.);
#2035=ORIENTED_EDGE('',*,*,#1460,.T.);
#2036=ORIENTED_EDGE('',*,*,#1458,.T.);
#2037=ORIENTED_EDGE('',*,*,#1441,.T.);
#2038=ORIENTED_EDGE('',*,*,#1455,.F.);
#2039=ORIENTED_EDGE('',*,*,#1457,.F.);
#2040=ORIENTED_EDGE('',*,*,#1459,.F.);
#2041=ORIENTED_EDGE('',*,*,#1460,.F.);
#2042=ORIENTED_EDGE('',*,*,#1450,.F.);
#2043=ORIENTED_EDGE('',*,*,#1453,.F.);
#2044=ORIENTED_EDGE('',*,*,#1438,.T.);
#2045=CYLINDRICAL_SURFACE('',#2311,0.4);
#2046=CYLINDRICAL_SURFACE('',#2316,0.25);
#2047=CYLINDRICAL_SURFACE('',#2320,0.25);
#2048=CYLINDRICAL_SURFACE('',#2324,0.25);
#2049=CYLINDRICAL_SURFACE('',#2328,0.25);
#2050=CYLINDRICAL_SURFACE('',#2334,0.4);
#2051=CYLINDRICAL_SURFACE('',#2340,0.93);
#2052=CYLINDRICAL_SURFACE('',#2344,0.49);
#2053=CYLINDRICAL_SURFACE('',#2351,0.25);
#2054=CYLINDRICAL_SURFACE('',#2353,0.25);
#2055=CYLINDRICAL_SURFACE('',#2355,0.4);
#2056=CYLINDRICAL_SURFACE('',#2364,0.2);
#2057=CYLINDRICAL_SURFACE('',#2367,0.79);
#2058=CYLINDRICAL_SURFACE('',#2369,0.93);
#2059=CYLINDRICAL_SURFACE('',#2380,0.199999999999999);
#2060=CYLINDRICAL_SURFACE('',#2384,0.685);
#2061=CYLINDRICAL_SURFACE('',#2388,0.0250000000000004);
#2062=CYLINDRICAL_SURFACE('',#2390,0.93);
#2063=CYLINDRICAL_SURFACE('',#2403,1.7);
#2064=CYLINDRICAL_SURFACE('',#2405,0.55);
#2065=CYLINDRICAL_SURFACE('',#2411,0.33);
#2066=CYLINDRICAL_SURFACE('',#2415,0.33);
#2067=CYLINDRICAL_SURFACE('',#2419,0.55);
#2068=CYLINDRICAL_SURFACE('',#2433,0.33);
#2069=CYLINDRICAL_SURFACE('',#2441,0.55);
#2070=CYLINDRICAL_SURFACE('',#2444,0.33);
#2071=CYLINDRICAL_SURFACE('',#2448,0.33);
#2072=CYLINDRICAL_SURFACE('',#2451,0.55);
#2073=CYLINDRICAL_SURFACE('',#2454,0.33);
#2074=CYLINDRICAL_SURFACE('',#2457,0.33);
#2075=CYLINDRICAL_SURFACE('',#2459,0.33);
#2076=CYLINDRICAL_SURFACE('',#2478,1.065);
#2077=CYLINDRICAL_SURFACE('',#2484,1.065);
#2078=CYLINDRICAL_SURFACE('',#2490,0.79);
#2079=CYLINDRICAL_SURFACE('',#2496,0.3);
#2080=CYLINDRICAL_SURFACE('',#2500,0.6);
#2081=CYLINDRICAL_SURFACE('',#2511,2.);
#2082=CYLINDRICAL_SURFACE('',#2514,0.685);
#2083=CYLINDRICAL_SURFACE('',#2517,1.9);
#2084=CYLINDRICAL_SURFACE('',#2530,0.2942);
#2085=ADVANCED_FACE('',(#241),#2045,.F.);
#2086=ADVANCED_FACE('',(#242),#2046,.F.);
#2087=ADVANCED_FACE('',(#243),#164,.F.);
#2088=ADVANCED_FACE('',(#244),#2047,.F.);
#2089=ADVANCED_FACE('',(#245),#165,.F.);
#2090=ADVANCED_FACE('',(#246),#2048,.F.);
#2091=ADVANCED_FACE('',(#247),#166,.F.);
#2092=ADVANCED_FACE('',(#248),#2049,.F.);
#2093=ADVANCED_FACE('',(#249),#167,.F.);
#2094=ADVANCED_FACE('',(#250),#168,.T.);
#2095=ADVANCED_FACE('',(#251),#2050,.F.);
#2096=ADVANCED_FACE('',(#252),#169,.T.);
#2097=ADVANCED_FACE('',(#253),#2051,.F.);
#2098=ADVANCED_FACE('',(#254,#112),#170,.T.);
#2099=ADVANCED_FACE('',(#255),#2052,.F.);
#2100=ADVANCED_FACE('',(#256,#113),#171,.F.);
#2101=ADVANCED_FACE('',(#257,#114),#172,.T.);
#2102=ADVANCED_FACE('',(#258),#2053,.F.);
#2103=ADVANCED_FACE('',(#259),#2054,.F.);
#2104=ADVANCED_FACE('',(#260),#2055,.F.);
#2105=ADVANCED_FACE('',(#261,#115),#173,.F.);
#2106=ADVANCED_FACE('',(#262),#174,.T.);
#2107=ADVANCED_FACE('',(#263),#175,.T.);
#2108=ADVANCED_FACE('',(#264),#2056,.F.);
#2109=ADVANCED_FACE('',(#265),#176,.F.);
#2110=ADVANCED_FACE('',(#266),#2057,.F.);
#2111=ADVANCED_FACE('',(#267),#2058,.F.);
#2112=ADVANCED_FACE('',(#268,#116),#177,.F.);
#2113=ADVANCED_FACE('',(#269),#178,.T.);
#2114=ADVANCED_FACE('',(#270,#117),#179,.T.);
#2115=ADVANCED_FACE('',(#271),#180,.T.);
#2116=ADVANCED_FACE('',(#272,#118),#181,.T.);
#2117=ADVANCED_FACE('',(#273,#119),#182,.T.);
#2118=ADVANCED_FACE('',(#274,#120,#121,#122,#123),#183,.F.);
#2119=ADVANCED_FACE('',(#275),#2059,.F.);
#2120=ADVANCED_FACE('',(#276),#184,.F.);
#2121=ADVANCED_FACE('',(#277),#2060,.F.);
#2122=ADVANCED_FACE('',(#278,#124),#185,.F.);
#2123=ADVANCED_FACE('',(#279),#2061,.F.);
#2124=ADVANCED_FACE('',(#280),#2062,.F.);
#2125=ADVANCED_FACE('',(#281,#125),#186,.F.);
#2126=ADVANCED_FACE('',(#282),#187,.T.);
#2127=ADVANCED_FACE('',(#283),#188,.T.);
#2128=ADVANCED_FACE('',(#284,#126),#189,.T.);
#2129=ADVANCED_FACE('',(#285,#127),#190,.T.);
#2130=ADVANCED_FACE('',(#286),#191,.T.);
#2131=ADVANCED_FACE('',(#287),#192,.F.);
#2132=ADVANCED_FACE('',(#288),#193,.F.);
#2133=ADVANCED_FACE('',(#289),#2063,.F.);
#2134=ADVANCED_FACE('',(#290),#2064,.F.);
#2135=ADVANCED_FACE('',(#291),#2065,.F.);
#2136=ADVANCED_FACE('',(#292),#2066,.F.);
#2137=ADVANCED_FACE('',(#293),#2067,.F.);
#2138=ADVANCED_FACE('',(#294),#194,.F.);
#2139=ADVANCED_FACE('',(#295,#128,#129,#130,#131),#195,.T.);
#2140=ADVANCED_FACE('',(#296),#2068,.F.);
#2141=ADVANCED_FACE('',(#297,#132,#133,#134,#135),#196,.F.);
#2142=ADVANCED_FACE('',(#298),#2069,.F.);
#2143=ADVANCED_FACE('',(#299),#197,.F.);
#2144=ADVANCED_FACE('',(#300),#2070,.F.);
#2145=ADVANCED_FACE('',(#301),#198,.F.);
#2146=ADVANCED_FACE('',(#302),#199,.T.);
#2147=ADVANCED_FACE('',(#303),#2071,.F.);
#2148=ADVANCED_FACE('',(#304),#200,.T.);
#2149=ADVANCED_FACE('',(#305),#2072,.F.);
#2150=ADVANCED_FACE('',(#306),#2073,.F.);
#2151=ADVANCED_FACE('',(#307),#201,.T.);
#2152=ADVANCED_FACE('',(#308),#2074,.F.);
#2153=ADVANCED_FACE('',(#309),#2075,.F.);
#2154=ADVANCED_FACE('',(#310),#202,.T.);
#2155=ADVANCED_FACE('',(#311,#136),#203,.T.);
#2156=ADVANCED_FACE('',(#312,#137,#138,#139,#140),#204,.T.);
#2157=ADVANCED_FACE('',(#313,#141),#205,.T.);
#2158=ADVANCED_FACE('',(#314),#206,.T.);
#2159=ADVANCED_FACE('',(#315,#142,#143,#144,#145),#207,.F.);
#2160=ADVANCED_FACE('',(#316,#146),#208,.F.);
#2161=ADVANCED_FACE('',(#317,#147),#209,.T.);
#2162=ADVANCED_FACE('',(#318),#210,.T.);
#2163=ADVANCED_FACE('',(#319),#211,.T.);
#2164=ADVANCED_FACE('',(#320),#212,.T.);
#2165=ADVANCED_FACE('',(#321),#213,.T.);
#2166=ADVANCED_FACE('',(#322),#214,.T.);
#2167=ADVANCED_FACE('',(#323),#215,.T.);
#2168=ADVANCED_FACE('',(#324),#2076,.T.);
#2169=ADVANCED_FACE('',(#325,#148),#216,.T.);
#2170=ADVANCED_FACE('',(#326),#70,.T.);
#2171=ADVANCED_FACE('',(#327),#2077,.T.);
#2172=ADVANCED_FACE('',(#328),#71,.T.);
#2173=ADVANCED_FACE('',(#329,#149),#217,.T.);
#2174=ADVANCED_FACE('',(#330),#2078,.F.);
#2175=ADVANCED_FACE('',(#331),#72,.T.);
#2176=ADVANCED_FACE('',(#332),#73,.T.);
#2177=ADVANCED_FACE('',(#333),#2079,.T.);
#2178=ADVANCED_FACE('',(#334,#150),#218,.T.);
#2179=ADVANCED_FACE('',(#335),#2080,.T.);
#2180=ADVANCED_FACE('',(#336),#219,.T.);
#2181=ADVANCED_FACE('',(#337),#69,.T.);
#2182=ADVANCED_FACE('',(#338,#151),#220,.T.);
#2183=ADVANCED_FACE('',(#339),#2081,.T.);
#2184=ADVANCED_FACE('',(#340),#221,.F.);
#2185=ADVANCED_FACE('',(#341),#2082,.T.);
#2186=ADVANCED_FACE('',(#342),#222,.T.);
#2187=ADVANCED_FACE('',(#343),#2083,.T.);
#2188=ADVANCED_FACE('',(#344),#223,.T.);
#2189=ADVANCED_FACE('',(#345),#224,.F.);
#2190=ADVANCED_FACE('',(#346),#225,.T.);
#2191=ADVANCED_FACE('',(#347),#226,.T.);
#2192=ADVANCED_FACE('',(#348),#227,.T.);
#2193=ADVANCED_FACE('',(#349),#228,.T.);
#2194=ADVANCED_FACE('',(#350),#229,.T.);
#2195=ADVANCED_FACE('',(#351),#230,.T.);
#2196=ADVANCED_FACE('',(#352),#231,.F.);
#2197=ADVANCED_FACE('',(#353),#2084,.T.);
#2198=ADVANCED_FACE('',(#354),#74,.T.);
#2199=ADVANCED_FACE('',(#355),#232,.T.);
#2200=ADVANCED_FACE('',(#356),#75,.T.);
#2201=ADVANCED_FACE('',(#357),#233,.T.);
#2202=ADVANCED_FACE('',(#358),#234,.T.);
#2203=ADVANCED_FACE('',(#359),#235,.T.);
#2204=ADVANCED_FACE('',(#360),#236,.T.);
#2205=ADVANCED_FACE('',(#361),#237,.T.);
#2206=ADVANCED_FACE('',(#362),#238,.T.);
#2207=ADVANCED_FACE('',(#363),#239,.T.);
#2208=ADVANCED_FACE('',(#364,#152),#240,.F.);
#2209=CLOSED_SHELL('',(#2085,#2086,#2087,#2088,#2089,#2090,#2091,#2092,
#2093,#2094,#2095,#2096,#2097,#2098,#2099,#2100,#2101,#2102,#2103,#2104,
#2105,#2106,#2107,#2108,#2109,#2110,#2111,#2112,#2113,#2114,#2115,#2116,
#2117,#2118));
#2210=CLOSED_SHELL('',(#2119,#2120,#2121,#2122,#2123,#2124,#2125,#2126,
#2127,#2128,#2129,#2130,#2131));
#2211=CLOSED_SHELL('',(#2132,#2133,#2134,#2135,#2136,#2137,#2138,#2139,
#2140,#2141,#2142,#2143,#2144,#2145,#2146,#2147,#2148,#2149,#2150,#2151,
#2152,#2153,#2154,#2155,#2156,#2157,#2158,#2159));
#2212=CLOSED_SHELL('',(#2160,#2161,#2162,#2163,#2164,#2165,#2166,#2167,
#2168,#2169,#2170,#2171,#2172,#2173,#2174));
#2213=CLOSED_SHELL('',(#2175,#2176,#2177,#2178,#2179,#2180));
#2214=CLOSED_SHELL('',(#2181));
#2215=CLOSED_SHELL('',(#2182,#2183,#2184,#2185,#2186));
#2216=CLOSED_SHELL('',(#2187,#2188,#2189));
#2217=CLOSED_SHELL('',(#2190,#2191,#2192,#2193,#2194,#2195,#2196));
#2218=CLOSED_SHELL('',(#2197,#2198,#2199,#2200,#2201,#2202,#2203,#2204,
#2205,#2206,#2207,#2208));
#2219=DERIVED_UNIT_ELEMENT(#2235,1.);
#2220=DERIVED_UNIT_ELEMENT(#4045,-3.);
#2221=DERIVED_UNIT_ELEMENT(#2235,1.);
#2222=DERIVED_UNIT_ELEMENT(#4045,-3.);
#2223=DERIVED_UNIT_ELEMENT(#2235,1.);
#2224=DERIVED_UNIT_ELEMENT(#4045,-3.);
#2225=DERIVED_UNIT_ELEMENT(#2235,1.);
#2226=DERIVED_UNIT_ELEMENT(#4045,-3.);
#2227=DERIVED_UNIT_ELEMENT(#2235,1.);
#2228=DERIVED_UNIT_ELEMENT(#4045,-3.);
#2229=DERIVED_UNIT_ELEMENT(#2235,1.);
#2230=DERIVED_UNIT_ELEMENT(#4045,-3.);
#2231=DERIVED_UNIT_ELEMENT(#2235,1.);
#2232=DERIVED_UNIT_ELEMENT(#4045,-3.);
#2233=DERIVED_UNIT_ELEMENT(#2235,1.);
#2234=DERIVED_UNIT_ELEMENT(#4045,-3.);
#2235=(
MASS_UNIT()
NAMED_UNIT(*)
SI_UNIT(.KILO.,.GRAM.)
);
#2236=DERIVED_UNIT((#2219,#2220));
#2237=DERIVED_UNIT((#2221,#2222));
#2238=DERIVED_UNIT((#2223,#2224));
#2239=DERIVED_UNIT((#2225,#2226));
#2240=DERIVED_UNIT((#2227,#2228));
#2241=DERIVED_UNIT((#2229,#2230));
#2242=DERIVED_UNIT((#2231,#2232));
#2243=DERIVED_UNIT((#2233,#2234));
#2244=MEASURE_REPRESENTATION_ITEM('density measure',
POSITIVE_RATIO_MEASURE(7850.),#2236);
#2245=MEASURE_REPRESENTATION_ITEM('density measure',
POSITIVE_RATIO_MEASURE(7850.),#2237);
#2246=MEASURE_REPRESENTATION_ITEM('density measure',
POSITIVE_RATIO_MEASURE(7850.),#2238);
#2247=MEASURE_REPRESENTATION_ITEM('density measure',
POSITIVE_RATIO_MEASURE(7850.),#2239);
#2248=MEASURE_REPRESENTATION_ITEM('density measure',
POSITIVE_RATIO_MEASURE(7850.),#2240);
#2249=MEASURE_REPRESENTATION_ITEM('density measure',
POSITIVE_RATIO_MEASURE(7850.),#2241);
#2250=MEASURE_REPRESENTATION_ITEM('density measure',
POSITIVE_RATIO_MEASURE(7850.),#2242);
#2251=MEASURE_REPRESENTATION_ITEM('density measure',
POSITIVE_RATIO_MEASURE(7850.),#2243);
#2252=PROPERTY_DEFINITION_REPRESENTATION(#2292,#2268);
#2253=PROPERTY_DEFINITION_REPRESENTATION(#2293,#2269);
#2254=PROPERTY_DEFINITION_REPRESENTATION(#2294,#2270);
#2255=PROPERTY_DEFINITION_REPRESENTATION(#2295,#2271);
#2256=PROPERTY_DEFINITION_REPRESENTATION(#2296,#2272);
#2257=PROPERTY_DEFINITION_REPRESENTATION(#2297,#2273);
#2258=PROPERTY_DEFINITION_REPRESENTATION(#2298,#2274);
#2259=PROPERTY_DEFINITION_REPRESENTATION(#2299,#2275);
#2260=PROPERTY_DEFINITION_REPRESENTATION(#2300,#2276);
#2261=PROPERTY_DEFINITION_REPRESENTATION(#2301,#2277);
#2262=PROPERTY_DEFINITION_REPRESENTATION(#2302,#2278);
#2263=PROPERTY_DEFINITION_REPRESENTATION(#2303,#2279);
#2264=PROPERTY_DEFINITION_REPRESENTATION(#2304,#2280);
#2265=PROPERTY_DEFINITION_REPRESENTATION(#2305,#2281);
#2266=PROPERTY_DEFINITION_REPRESENTATION(#2306,#2282);
#2267=PROPERTY_DEFINITION_REPRESENTATION(#2307,#2283);
#2268=REPRESENTATION('material name',(#2284),#4035);
#2269=REPRESENTATION('density',(#2244),#4035);
#2270=REPRESENTATION('material name',(#2285),#4036);
#2271=REPRESENTATION('density',(#2245),#4036);
#2272=REPRESENTATION('material name',(#2286),#4037);
#2273=REPRESENTATION('density',(#2246),#4037);
#2274=REPRESENTATION('material name',(#2287),#4038);
#2275=REPRESENTATION('density',(#2247),#4038);
#2276=REPRESENTATION('material name',(#2288),#4039);
#2277=REPRESENTATION('density',(#2248),#4039);
#2278=REPRESENTATION('material name',(#2289),#4040);
#2279=REPRESENTATION('density',(#2249),#4040);
#2280=REPRESENTATION('material name',(#2290),#4041);
#2281=REPRESENTATION('density',(#2250),#4041);
#2282=REPRESENTATION('material name',(#2291),#4042);
#2283=REPRESENTATION('density',(#2251),#4042);
#2284=DESCRIPTIVE_REPRESENTATION_ITEM('Steel','Steel');
#2285=DESCRIPTIVE_REPRESENTATION_ITEM('Steel','Steel');
#2286=DESCRIPTIVE_REPRESENTATION_ITEM('Steel','Steel');
#2287=DESCRIPTIVE_REPRESENTATION_ITEM('Steel','Steel');
#2288=DESCRIPTIVE_REPRESENTATION_ITEM('Steel','Steel');
#2289=DESCRIPTIVE_REPRESENTATION_ITEM('Steel','Steel');
#2290=DESCRIPTIVE_REPRESENTATION_ITEM('Steel','Steel');
#2291=DESCRIPTIVE_REPRESENTATION_ITEM('Steel','Steel');
#2292=PROPERTY_DEFINITION('material property','material name',#4094);
#2293=PROPERTY_DEFINITION('material property','density of part',#4094);
#2294=PROPERTY_DEFINITION('material property','material name',#4095);
#2295=PROPERTY_DEFINITION('material property','density of part',#4095);
#2296=PROPERTY_DEFINITION('material property','material name',#4096);
#2297=PROPERTY_DEFINITION('material property','density of part',#4096);
#2298=PROPERTY_DEFINITION('material property','material name',#4097);
#2299=PROPERTY_DEFINITION('material property','density of part',#4097);
#2300=PROPERTY_DEFINITION('material property','material name',#4098);
#2301=PROPERTY_DEFINITION('material property','density of part',#4098);
#2302=PROPERTY_DEFINITION('material property','material name',#4099);
#2303=PROPERTY_DEFINITION('material property','density of part',#4099);
#2304=PROPERTY_DEFINITION('material property','material name',#4100);
#2305=PROPERTY_DEFINITION('material property','density of part',#4100);
#2306=PROPERTY_DEFINITION('material property','material name',#4101);
#2307=PROPERTY_DEFINITION('material property','density of part',#4101);
#2308=AXIS2_PLACEMENT_3D('',#3232,#2559,#2560);
#2309=AXIS2_PLACEMENT_3D('',#3233,#2561,#2562);
#2310=AXIS2_PLACEMENT_3D('',#3234,#2563,#2564);
#2311=AXIS2_PLACEMENT_3D('',#3235,#2565,#2566);
#2312=AXIS2_PLACEMENT_3D('',#3240,#2568,#2569);
#2313=AXIS2_PLACEMENT_3D('',#3242,#2570,#2571);
#2314=AXIS2_PLACEMENT_3D('',#3244,#2572,#2573);
#2315=AXIS2_PLACEMENT_3D('',#3245,#2574,#2575);
#2316=AXIS2_PLACEMENT_3D('',#3246,#2576,#2577);
#2317=AXIS2_PLACEMENT_3D('',#3248,#2578,#2579);
#2318=AXIS2_PLACEMENT_3D('',#3251,#2581,#2582);
#2319=AXIS2_PLACEMENT_3D('',#3252,#2583,#2584);
#2320=AXIS2_PLACEMENT_3D('',#3253,#2585,#2586);
#2321=AXIS2_PLACEMENT_3D('',#3255,#2587,#2588);
#2322=AXIS2_PLACEMENT_3D('',#3258,#2590,#2591);
#2323=AXIS2_PLACEMENT_3D('',#3259,#2592,#2593);
#2324=AXIS2_PLACEMENT_3D('',#3260,#2594,#2595);
#2325=AXIS2_PLACEMENT_3D('',#3262,#2596,#2597);
#2326=AXIS2_PLACEMENT_3D('',#3265,#2599,#2600);
#2327=AXIS2_PLACEMENT_3D('',#3266,#2601,#2602);
#2328=AXIS2_PLACEMENT_3D('',#3267,#2603,#2604);
#2329=AXIS2_PLACEMENT_3D('',#3269,#2605,#2606);
#2330=AXIS2_PLACEMENT_3D('',#3272,#2608,#2609);
#2331=AXIS2_PLACEMENT_3D('',#3273,#2610,#2611);
#2332=AXIS2_PLACEMENT_3D('',#3274,#2612,#2613);
#2333=AXIS2_PLACEMENT_3D('',#3279,#2615,#2616);
#2334=AXIS2_PLACEMENT_3D('',#3281,#2618,#2619);
#2335=AXIS2_PLACEMENT_3D('',#3285,#2621,#2622);
#2336=AXIS2_PLACEMENT_3D('',#3307,#2624,#2625);
#2337=AXIS2_PLACEMENT_3D('',#3308,#2626,#2627);
#2338=AXIS2_PLACEMENT_3D('',#3311,#2629,#2630);
#2339=AXIS2_PLACEMENT_3D('',#3312,#2631,#2632);
#2340=AXIS2_PLACEMENT_3D('',#3316,#2635,#2636);
#2341=AXIS2_PLACEMENT_3D('',#3318,#2637,#2638);
#2342=AXIS2_PLACEMENT_3D('',#3321,#2640,#2641);
#2343=AXIS2_PLACEMENT_3D('',#3322,#2642,#2643);
#2344=AXIS2_PLACEMENT_3D('',#3323,#2644,#2645);
#2345=AXIS2_PLACEMENT_3D('',#3325,#2646,#2647);
#2346=AXIS2_PLACEMENT_3D('',#3328,#2649,#2650);
#2347=AXIS2_PLACEMENT_3D('',#3329,#2651,#2652);
#2348=AXIS2_PLACEMENT_3D('',#3331,#2653,#2654);
#2349=AXIS2_PLACEMENT_3D('',#3332,#2655,#2656);
#2350=AXIS2_PLACEMENT_3D('',#3334,#2657,#2658);
#2351=AXIS2_PLACEMENT_3D('',#3335,#2659,#2660);
#2352=AXIS2_PLACEMENT_3D('',#3337,#2661,#2662);
#2353=AXIS2_PLACEMENT_3D('',#3339,#2664,#2665);
#2354=AXIS2_PLACEMENT_3D('',#3342,#2667,#2668);
#2355=AXIS2_PLACEMENT_3D('',#3343,#2669,#2670);
#2356=AXIS2_PLACEMENT_3D('',#3344,#2671,#2672);
#2357=AXIS2_PLACEMENT_3D('',#3345,#2673,#2674);
#2358=AXIS2_PLACEMENT_3D('',#3346,#2675,#2676);
#2359=AXIS2_PLACEMENT_3D('',#3347,#2677,#2678);
#2360=AXIS2_PLACEMENT_3D('',#3349,#2679,#2680);
#2361=AXIS2_PLACEMENT_3D('',#3350,#2681,#2682);
#2362=AXIS2_PLACEMENT_3D('',#3351,#2683,#2684);
#2363=AXIS2_PLACEMENT_3D('',#3355,#2686,#2687);
#2364=AXIS2_PLACEMENT_3D('',#3356,#2688,#2689);
#2365=AXIS2_PLACEMENT_3D('',#3392,#2693,#2694);
#2366=AXIS2_PLACEMENT_3D('',#3393,#2695,#2696);
#2367=AXIS2_PLACEMENT_3D('',#3394,#2697,#2698);
#2368=AXIS2_PLACEMENT_3D('',#3396,#2699,#2700);
#2369=AXIS2_PLACEMENT_3D('',#3398,#2702,#2703);
#2370=AXIS2_PLACEMENT_3D('',#3400,#2704,#2705);
#2371=AXIS2_PLACEMENT_3D('',#3403,#2707,#2708);
#2372=AXIS2_PLACEMENT_3D('',#3404,#2709,#2710);
#2373=AXIS2_PLACEMENT_3D('',#3405,#2711,#2712);
#2374=AXIS2_PLACEMENT_3D('',#3414,#2717,#2718);
#2375=AXIS2_PLACEMENT_3D('',#3420,#2722,#2723);
#2376=AXIS2_PLACEMENT_3D('',#3426,#2727,#2728);
#2377=AXIS2_PLACEMENT_3D('',#3429,#2731,#2732);
#2378=AXIS2_PLACEMENT_3D('',#3430,#2733,#2734);
#2379=AXIS2_PLACEMENT_3D('',#3431,#2735,#2736);
#2380=AXIS2_PLACEMENT_3D('',#3432,#2737,#2738);
#2381=AXIS2_PLACEMENT_3D('',#3434,#2739,#2740);
#2382=AXIS2_PLACEMENT_3D('',#3437,#2742,#2743);
#2383=AXIS2_PLACEMENT_3D('',#3438,#2744,#2745);
#2384=AXIS2_PLACEMENT_3D('',#3439,#2746,#2747);
#2385=AXIS2_PLACEMENT_3D('',#3441,#2748,#2749);
#2386=AXIS2_PLACEMENT_3D('',#3468,#2752,#2753);
#2387=AXIS2_PLACEMENT_3D('',#3490,#2754,#2755);
#2388=AXIS2_PLACEMENT_3D('',#3491,#2756,#2757);
#2389=AXIS2_PLACEMENT_3D('',#3493,#2758,#2759);
#2390=AXIS2_PLACEMENT_3D('',#3495,#2761,#2762);
#2391=AXIS2_PLACEMENT_3D('',#3497,#2763,#2764);
#2392=AXIS2_PLACEMENT_3D('',#3500,#2766,#2767);
#2393=AXIS2_PLACEMENT_3D('',#3501,#2768,#2769);
#2394=AXIS2_PLACEMENT_3D('',#3502,#2770,#2771);
#2395=AXIS2_PLACEMENT_3D('',#3511,#2776,#2777);
#2396=AXIS2_PLACEMENT_3D('',#3517,#2781,#2782);
#2397=AXIS2_PLACEMENT_3D('',#3523,#2786,#2787);
#2398=AXIS2_PLACEMENT_3D('',#3526,#2790,#2791);
#2399=AXIS2_PLACEMENT_3D('',#3527,#2792,#2793);
#2400=AXIS2_PLACEMENT_3D('',#3528,#2794,#2795);
#2401=AXIS2_PLACEMENT_3D('',#3529,#2796,#2797);
#2402=AXIS2_PLACEMENT_3D('',#3534,#2799,#2800);
#2403=AXIS2_PLACEMENT_3D('',#3538,#2803,#2804);
#2404=AXIS2_PLACEMENT_3D('',#3580,#2807,#2808);
#2405=AXIS2_PLACEMENT_3D('',#3622,#2811,#2812);
#2406=AXIS2_PLACEMENT_3D('',#3627,#2814,#2815);
#2407=AXIS2_PLACEMENT_3D('',#3631,#2817,#2818);
#2408=AXIS2_PLACEMENT_3D('',#3634,#2820,#2821);
#2409=AXIS2_PLACEMENT_3D('',#3635,#2822,#2823);
#2410=AXIS2_PLACEMENT_3D('',#3636,#2824,#2825);
#2411=AXIS2_PLACEMENT_3D('',#3637,#2826,#2827);
#2412=AXIS2_PLACEMENT_3D('',#3639,#2828,#2829);
#2413=AXIS2_PLACEMENT_3D('',#3642,#2831,#2832);
#2414=AXIS2_PLACEMENT_3D('',#3643,#2833,#2834);
#2415=AXIS2_PLACEMENT_3D('',#3644,#2835,#2836);
#2416=AXIS2_PLACEMENT_3D('',#3646,#2837,#2838);
#2417=AXIS2_PLACEMENT_3D('',#3649,#2840,#2841);
#2418=AXIS2_PLACEMENT_3D('',#3650,#2842,#2843);
#2419=AXIS2_PLACEMENT_3D('',#3651,#2844,#2845);
#2420=AXIS2_PLACEMENT_3D('',#3656,#2847,#2848);
#2421=AXIS2_PLACEMENT_3D('',#3659,#2850,#2851);
#2422=AXIS2_PLACEMENT_3D('',#3661,#2852,#2853);
#2423=AXIS2_PLACEMENT_3D('',#3664,#2855,#2856);
#2424=AXIS2_PLACEMENT_3D('',#3665,#2857,#2858);
#2425=AXIS2_PLACEMENT_3D('',#3671,#2862,#2863);
#2426=AXIS2_PLACEMENT_3D('',#3680,#2868,#2869);
#2427=AXIS2_PLACEMENT_3D('',#3682,#2870,#2871);
#2428=AXIS2_PLACEMENT_3D('',#3689,#2875,#2876);
#2429=AXIS2_PLACEMENT_3D('',#3691,#2877,#2878);
#2430=AXIS2_PLACEMENT_3D('',#3693,#2879,#2880);
#2431=AXIS2_PLACEMENT_3D('',#3695,#2881,#2882);
#2432=AXIS2_PLACEMENT_3D('',#3697,#2883,#2884);
#2433=AXIS2_PLACEMENT_3D('',#3698,#2885,#2886);
#2434=AXIS2_PLACEMENT_3D('',#3700,#2887,#2888);
#2435=AXIS2_PLACEMENT_3D('',#3702,#2890,#2891);
#2436=AXIS2_PLACEMENT_3D('',#3704,#2892,#2893);
#2437=AXIS2_PLACEMENT_3D('',#3706,#2894,#2895);
#2438=AXIS2_PLACEMENT_3D('',#3714,#2899,#2900);
#2439=AXIS2_PLACEMENT_3D('',#3722,#2905,#2906);
#2440=AXIS2_PLACEMENT_3D('',#3724,#2907,#2908);
#2441=AXIS2_PLACEMENT_3D('',#3725,#2909,#2910);
#2442=AXIS2_PLACEMENT_3D('',#3729,#2913,#2914);
#2443=AXIS2_PLACEMENT_3D('',#3730,#2915,#2916);
#2444=AXIS2_PLACEMENT_3D('',#3732,#2918,#2919);
#2445=AXIS2_PLACEMENT_3D('',#3734,#2920,#2921);
#2446=AXIS2_PLACEMENT_3D('',#3736,#2923,#2924);
#2447=AXIS2_PLACEMENT_3D('',#3738,#2926,#2927);
#2448=AXIS2_PLACEMENT_3D('',#3740,#2929,#2930);
#2449=AXIS2_PLACEMENT_3D('',#3742,#2931,#2932);
#2450=AXIS2_PLACEMENT_3D('',#3744,#2934,#2935);
#2451=AXIS2_PLACEMENT_3D('',#3746,#2937,#2938);
#2452=AXIS2_PLACEMENT_3D('',#3750,#2941,#2942);
#2453=AXIS2_PLACEMENT_3D('',#3751,#2943,#2944);
#2454=AXIS2_PLACEMENT_3D('',#3752,#2945,#2946);
#2455=AXIS2_PLACEMENT_3D('',#3754,#2947,#2948);
#2456=AXIS2_PLACEMENT_3D('',#3756,#2950,#2951);
#2457=AXIS2_PLACEMENT_3D('',#3758,#2953,#2954);
#2458=AXIS2_PLACEMENT_3D('',#3761,#2956,#2957);
#2459=AXIS2_PLACEMENT_3D('',#3762,#2958,#2959);
#2460=AXIS2_PLACEMENT_3D('',#3765,#2961,#2962);
#2461=AXIS2_PLACEMENT_3D('',#3766,#2963,#2964);
#2462=AXIS2_PLACEMENT_3D('',#3775,#2969,#2970);
#2463=AXIS2_PLACEMENT_3D('',#3781,#2974,#2975);
#2464=AXIS2_PLACEMENT_3D('',#3786,#2979,#2980);
#2465=AXIS2_PLACEMENT_3D('',#3790,#2983,#2984);
#2466=AXIS2_PLACEMENT_3D('',#3792,#2986,#2987);
#2467=AXIS2_PLACEMENT_3D('',#3793,#2988,#2989);
#2468=AXIS2_PLACEMENT_3D('',#3794,#2990,#2991);
#2469=AXIS2_PLACEMENT_3D('',#3808,#2998,#2999);
#2470=AXIS2_PLACEMENT_3D('',#3809,#3000,#3001);
#2471=AXIS2_PLACEMENT_3D('',#3823,#3008,#3009);
#2472=AXIS2_PLACEMENT_3D('',#3824,#3010,#3011);
#2473=AXIS2_PLACEMENT_3D('',#3827,#3014,#3015);
#2474=AXIS2_PLACEMENT_3D('',#3829,#3017,#3018);
#2475=AXIS2_PLACEMENT_3D('',#3831,#3020,#3021);
#2476=AXIS2_PLACEMENT_3D('',#3833,#3023,#3024);
#2477=AXIS2_PLACEMENT_3D('',#3835,#3026,#3027);
#2478=AXIS2_PLACEMENT_3D('',#3836,#3028,#3029);
#2479=AXIS2_PLACEMENT_3D('',#3839,#3031,#3032);
#2480=AXIS2_PLACEMENT_3D('',#3840,#3033,#3034);
#2481=AXIS2_PLACEMENT_3D('',#3842,#3035,#3036);
#2482=AXIS2_PLACEMENT_3D('',#3844,#3037,#3038);
#2483=AXIS2_PLACEMENT_3D('',#3845,#3039,#3040);
#2484=AXIS2_PLACEMENT_3D('',#3847,#3042,#3043);
#2485=AXIS2_PLACEMENT_3D('',#3849,#3044,#3045);
#2486=AXIS2_PLACEMENT_3D('',#3851,#3047,#3048);
#2487=AXIS2_PLACEMENT_3D('',#3853,#3049,#3050);
#2488=AXIS2_PLACEMENT_3D('',#3855,#3052,#3053);
#2489=AXIS2_PLACEMENT_3D('',#3857,#3054,#3055);
#2490=AXIS2_PLACEMENT_3D('',#3858,#3056,#3057);
#2491=AXIS2_PLACEMENT_3D('',#3860,#3059,#3060);
#2492=AXIS2_PLACEMENT_3D('',#3861,#3061,#3062);
#2493=AXIS2_PLACEMENT_3D('',#3863,#3063,#3064);
#2494=AXIS2_PLACEMENT_3D('',#3866,#3066,#3067);
#2495=AXIS2_PLACEMENT_3D('',#3868,#3068,#3069);
#2496=AXIS2_PLACEMENT_3D('',#3870,#3071,#3072);
#2497=AXIS2_PLACEMENT_3D('',#3872,#3073,#3074);
#2498=AXIS2_PLACEMENT_3D('',#3874,#3076,#3077);
#2499=AXIS2_PLACEMENT_3D('',#3876,#3078,#3079);
#2500=AXIS2_PLACEMENT_3D('',#3877,#3080,#3081);
#2501=AXIS2_PLACEMENT_3D('',#3879,#3082,#3083);
#2502=AXIS2_PLACEMENT_3D('',#3881,#3085,#3086);
#2503=AXIS2_PLACEMENT_3D('',#3882,#3087,#3088);
#2504=AXIS2_PLACEMENT_3D('',#3883,#3089,#3090);
#2505=AXIS2_PLACEMENT_3D('',#3885,#3091,#3092);
#2506=AXIS2_PLACEMENT_3D('',#3886,#3093,#3094);
#2507=AXIS2_PLACEMENT_3D('',#3887,#3095,#3096);
#2508=AXIS2_PLACEMENT_3D('',#3888,#3097,#3098);
#2509=AXIS2_PLACEMENT_3D('',#3890,#3099,#3100);
#2510=AXIS2_PLACEMENT_3D('',#3892,#3101,#3102);
#2511=AXIS2_PLACEMENT_3D('',#3893,#3103,#3104);
#2512=AXIS2_PLACEMENT_3D('',#3896,#3106,#3107);
#2513=AXIS2_PLACEMENT_3D('',#3897,#3108,#3109);
#2514=AXIS2_PLACEMENT_3D('',#3898,#3110,#3111);
#2515=AXIS2_PLACEMENT_3D('',#3900,#3112,#3113);
#2516=AXIS2_PLACEMENT_3D('',#3902,#3115,#3116);
#2517=AXIS2_PLACEMENT_3D('',#3903,#3117,#3118);
#2518=AXIS2_PLACEMENT_3D('',#3905,#3119,#3120);
#2519=AXIS2_PLACEMENT_3D('',#3908,#3122,#3123);
#2520=AXIS2_PLACEMENT_3D('',#3909,#3124,#3125);
#2521=AXIS2_PLACEMENT_3D('',#3910,#3126,#3127);
#2522=AXIS2_PLACEMENT_3D('',#3911,#3128,#3129);
#2523=AXIS2_PLACEMENT_3D('',#3920,#3134,#3135);
#2524=AXIS2_PLACEMENT_3D('',#3926,#3139,#3140);
#2525=AXIS2_PLACEMENT_3D('',#3932,#3144,#3145);
#2526=AXIS2_PLACEMENT_3D('',#3938,#3149,#3150);
#2527=AXIS2_PLACEMENT_3D('',#3941,#3153,#3154);
#2528=AXIS2_PLACEMENT_3D('',#3942,#3155,#3156);
#2529=AXIS2_PLACEMENT_3D('',#3943,#3157,#3158);
#2530=AXIS2_PLACEMENT_3D('',#3944,#3159,#3160);
#2531=AXIS2_PLACEMENT_3D('',#3946,#3161,#3162);
#2532=AXIS2_PLACEMENT_3D('',#3949,#3164,#3165);
#2533=AXIS2_PLACEMENT_3D('',#3950,#3166,#3167);
#2534=AXIS2_PLACEMENT_3D('',#3952,#3168,#3169);
#2535=AXIS2_PLACEMENT_3D('',#3954,#3171,#3172);
#2536=AXIS2_PLACEMENT_3D('',#3955,#3173,#3174);
#2537=AXIS2_PLACEMENT_3D('',#3957,#3175,#3176);
#2538=AXIS2_PLACEMENT_3D('',#3983,#3178,#3179);
#2539=AXIS2_PLACEMENT_3D('',#3989,#3183,#3184);
#2540=AXIS2_PLACEMENT_3D('',#3993,#3187,#3188);
#2541=AXIS2_PLACEMENT_3D('',#3997,#3191,#3192);
#2542=AXIS2_PLACEMENT_3D('',#4001,#3195,#3196);
#2543=AXIS2_PLACEMENT_3D('',#4005,#3199,#3200);
#2544=AXIS2_PLACEMENT_3D('',#4007,#3202,#3203);
#2545=AXIS2_PLACEMENT_3D('',#4008,#3204,#3205);
#2546=AXIS2_PLACEMENT_3D('',#4009,#3206,#3207);
#2547=AXIS2_PLACEMENT_3D('',#4010,#3208,#3209);
#2548=AXIS2_PLACEMENT_3D('',#4011,#3210,#3211);
#2549=AXIS2_PLACEMENT_3D('',#4012,#3212,#3213);
#2550=AXIS2_PLACEMENT_3D('',#4013,#3214,#3215);
#2551=AXIS2_PLACEMENT_3D('',#4014,#3216,#3217);
#2552=AXIS2_PLACEMENT_3D('',#4015,#3218,#3219);
#2553=AXIS2_PLACEMENT_3D('',#4016,#3220,#3221);
#2554=AXIS2_PLACEMENT_3D('',#4017,#3222,#3223);
#2555=AXIS2_PLACEMENT_3D('',#4018,#3224,#3225);
#2556=AXIS2_PLACEMENT_3D('',#4019,#3226,#3227);
#2557=AXIS2_PLACEMENT_3D('',#4020,#3228,#3229);
#2558=AXIS2_PLACEMENT_3D('',#4021,#3230,#3231);
#2559=DIRECTION('axis',(0.,0.,1.));
#2560=DIRECTION('refdir',(1.,0.,0.));
#2561=DIRECTION('axis',(0.,0.,1.));
#2562=DIRECTION('refdir',(1.,0.,0.));
#2563=DIRECTION('axis',(0.,0.,1.));
#2564=DIRECTION('refdir',(1.,0.,0.));
#2565=DIRECTION('center_axis',(0.,0.,1.));
#2566=DIRECTION('ref_axis',(1.,0.,0.));
#2567=DIRECTION('',(0.,0.,1.));
#2568=DIRECTION('center_axis',(0.,0.,1.));
#2569=DIRECTION('ref_axis',(1.,0.,0.));
#2570=DIRECTION('center_axis',(0.707106781186548,0.,0.707106781186547));
#2571=DIRECTION('ref_axis',(0.707106781186547,0.,-0.707106781186548));
#2572=DIRECTION('center_axis',(0.707106781186548,0.,-0.707106781186547));
#2573=DIRECTION('ref_axis',(-0.707106781186547,0.,-0.707106781186548));
#2574=DIRECTION('center_axis',(0.,0.,1.));
#2575=DIRECTION('ref_axis',(1.,0.,0.));
#2576=DIRECTION('center_axis',(0.,0.,1.));
#2577=DIRECTION('ref_axis',(1.,0.,0.));
#2578=DIRECTION('center_axis',(0.,0.,1.));
#2579=DIRECTION('ref_axis',(1.,0.,0.));
#2580=DIRECTION('',(0.,0.,1.));
#2581=DIRECTION('center_axis',(0.,0.,1.));
#2582=DIRECTION('ref_axis',(1.,0.,0.));
#2583=DIRECTION('center_axis',(0.,0.,1.));
#2584=DIRECTION('ref_axis',(1.,0.,0.));
#2585=DIRECTION('center_axis',(0.,0.,1.));
#2586=DIRECTION('ref_axis',(1.,0.,0.));
#2587=DIRECTION('center_axis',(0.,0.,1.));
#2588=DIRECTION('ref_axis',(1.,0.,0.));
#2589=DIRECTION('',(0.,0.,1.));
#2590=DIRECTION('center_axis',(0.,0.,1.));
#2591=DIRECTION('ref_axis',(1.,0.,0.));
#2592=DIRECTION('center_axis',(0.,0.,1.));
#2593=DIRECTION('ref_axis',(1.,0.,0.));
#2594=DIRECTION('center_axis',(0.,0.,1.));
#2595=DIRECTION('ref_axis',(1.,0.,0.));
#2596=DIRECTION('center_axis',(0.,0.,1.));
#2597=DIRECTION('ref_axis',(1.,0.,0.));
#2598=DIRECTION('',(0.,0.,1.));
#2599=DIRECTION('center_axis',(0.,0.,1.));
#2600=DIRECTION('ref_axis',(1.,0.,0.));
#2601=DIRECTION('center_axis',(0.,0.,1.));
#2602=DIRECTION('ref_axis',(1.,0.,0.));
#2603=DIRECTION('center_axis',(0.,0.,1.));
#2604=DIRECTION('ref_axis',(1.,0.,0.));
#2605=DIRECTION('center_axis',(0.,0.,1.));
#2606=DIRECTION('ref_axis',(1.,0.,0.));
#2607=DIRECTION('',(0.,0.,1.));
#2608=DIRECTION('center_axis',(0.,0.,1.));
#2609=DIRECTION('ref_axis',(1.,0.,0.));
#2610=DIRECTION('center_axis',(0.,0.,1.));
#2611=DIRECTION('ref_axis',(1.,0.,0.));
#2612=DIRECTION('center_axis',(1.,0.,0.));
#2613=DIRECTION('ref_axis',(0.,0.,-1.));
#2614=DIRECTION('',(0.,1.,0.));
#2615=DIRECTION('center_axis',(1.,0.,0.));
#2616=DIRECTION('ref_axis',(0.,0.,-1.));
#2617=DIRECTION('',(0.,0.,-1.));
#2618=DIRECTION('center_axis',(1.,0.,0.));
#2619=DIRECTION('ref_axis',(0.,0.,-1.));
#2620=DIRECTION('',(1.,0.,0.));
#2621=DIRECTION('center_axis',(1.,0.,0.));
#2622=DIRECTION('ref_axis',(0.,0.,-1.));
#2623=DIRECTION('',(-1.,0.,0.));
#2624=DIRECTION('center_axis',(0.707106781186548,0.,0.707106781186547));
#2625=DIRECTION('ref_axis',(0.707106781186547,0.,-0.707106781186548));
#2626=DIRECTION('center_axis',(0.707106781186548,0.,-0.707106781186547));
#2627=DIRECTION('ref_axis',(-0.707106781186547,0.,-0.707106781186548));
#2628=DIRECTION('',(1.,0.,0.));
#2629=DIRECTION('center_axis',(-1.,0.,0.));
#2630=DIRECTION('ref_axis',(0.,0.,-1.));
#2631=DIRECTION('center_axis',(1.,0.,0.));
#2632=DIRECTION('ref_axis',(0.,0.,-1.));
#2633=DIRECTION('',(0.,1.,0.));
#2634=DIRECTION('',(0.,0.,1.));
#2635=DIRECTION('center_axis',(1.,0.,0.));
#2636=DIRECTION('ref_axis',(0.,0.,-1.));
#2637=DIRECTION('center_axis',(1.,0.,0.));
#2638=DIRECTION('ref_axis',(0.,0.,-1.));
#2639=DIRECTION('',(1.,0.,0.));
#2640=DIRECTION('center_axis',(-1.,0.,0.));
#2641=DIRECTION('ref_axis',(0.,0.,-1.));
#2642=DIRECTION('center_axis',(1.,0.,0.));
#2643=DIRECTION('ref_axis',(0.,0.,-1.));
#2644=DIRECTION('center_axis',(0.,0.,1.));
#2645=DIRECTION('ref_axis',(1.,0.,0.));
#2646=DIRECTION('center_axis',(0.,0.,1.));
#2647=DIRECTION('ref_axis',(1.,0.,0.));
#2648=DIRECTION('',(0.,0.,1.));
#2649=DIRECTION('center_axis',(0.,0.,1.));
#2650=DIRECTION('ref_axis',(1.,0.,0.));
#2651=DIRECTION('center_axis',(0.,0.,1.));
#2652=DIRECTION('ref_axis',(1.,0.,0.));
#2653=DIRECTION('center_axis',(0.,0.,-1.));
#2654=DIRECTION('ref_axis',(1.,0.,0.));
#2655=DIRECTION('center_axis',(0.,0.,1.));
#2656=DIRECTION('ref_axis',(1.,0.,0.));
#2657=DIRECTION('center_axis',(0.,0.,1.));
#2658=DIRECTION('ref_axis',(1.,0.,0.));
#2659=DIRECTION('center_axis',(0.,0.,1.));
#2660=DIRECTION('ref_axis',(1.,0.,0.));
#2661=DIRECTION('center_axis',(0.,0.,1.));
#2662=DIRECTION('ref_axis',(1.,0.,0.));
#2663=DIRECTION('',(0.,0.,1.));
#2664=DIRECTION('center_axis',(0.,0.,1.));
#2665=DIRECTION('ref_axis',(1.,0.,0.));
#2666=DIRECTION('',(0.,0.,1.));
#2667=DIRECTION('center_axis',(0.,0.,-1.));
#2668=DIRECTION('ref_axis',(1.,0.,0.));
#2669=DIRECTION('center_axis',(0.,0.,1.));
#2670=DIRECTION('ref_axis',(1.,0.,0.));
#2671=DIRECTION('center_axis',(0.,0.,1.));
#2672=DIRECTION('ref_axis',(1.,0.,0.));
#2673=DIRECTION('center_axis',(0.,0.,1.));
#2674=DIRECTION('ref_axis',(1.,0.,0.));
#2675=DIRECTION('center_axis',(0.,0.,1.));
#2676=DIRECTION('ref_axis',(1.,0.,0.));
#2677=DIRECTION('center_axis',(0.,0.,1.));
#2678=DIRECTION('ref_axis',(1.,0.,0.));
#2679=DIRECTION('center_axis',(0.,0.,1.));
#2680=DIRECTION('ref_axis',(1.,0.,0.));
#2681=DIRECTION('center_axis',(0.,0.,1.));
#2682=DIRECTION('ref_axis',(1.,0.,0.));
#2683=DIRECTION('center_axis',(0.,0.,1.));
#2684=DIRECTION('ref_axis',(1.,0.,0.));
#2685=DIRECTION('',(0.,1.,0.));
#2686=DIRECTION('center_axis',(0.,0.,1.));
#2687=DIRECTION('ref_axis',(1.,0.,0.));
#2688=DIRECTION('center_axis',(0.,0.,1.));
#2689=DIRECTION('ref_axis',(1.,0.,0.));
#2690=DIRECTION('',(0.,0.,-1.));
#2691=DIRECTION('',(0.,0.,1.));
#2692=DIRECTION('',(0.,0.,1.));
#2693=DIRECTION('center_axis',(1.,0.,0.));
#2694=DIRECTION('ref_axis',(0.,0.,-1.));
#2695=DIRECTION('center_axis',(1.,0.,0.));
#2696=DIRECTION('ref_axis',(0.,0.,-1.));
#2697=DIRECTION('center_axis',(1.,0.,0.));
#2698=DIRECTION('ref_axis',(0.,0.,-1.));
#2699=DIRECTION('center_axis',(1.,0.,0.));
#2700=DIRECTION('ref_axis',(0.,0.,-1.));
#2701=DIRECTION('',(1.,0.,0.));
#2702=DIRECTION('center_axis',(1.,0.,0.));
#2703=DIRECTION('ref_axis',(0.,0.,-1.));
#2704=DIRECTION('center_axis',(1.,0.,0.));
#2705=DIRECTION('ref_axis',(0.,0.,-1.));
#2706=DIRECTION('',(1.,0.,0.));
#2707=DIRECTION('center_axis',(1.,0.,0.));
#2708=DIRECTION('ref_axis',(0.,0.,-1.));
#2709=DIRECTION('center_axis',(1.,0.,0.));
#2710=DIRECTION('ref_axis',(0.,0.,-1.));
#2711=DIRECTION('center_axis',(0.,1.,0.));
#2712=DIRECTION('ref_axis',(-1.,0.,0.));
#2713=DIRECTION('',(-1.,0.,0.));
#2714=DIRECTION('',(0.,0.,1.));
#2715=DIRECTION('',(-1.,0.,0.));
#2716=DIRECTION('',(0.,0.,1.));
#2717=DIRECTION('center_axis',(1.,0.,0.));
#2718=DIRECTION('ref_axis',(0.,1.,0.));
#2719=DIRECTION('',(0.,1.,0.));
#2720=DIRECTION('',(0.,1.,0.));
#2721=DIRECTION('',(0.,0.,1.));
#2722=DIRECTION('center_axis',(0.,-1.,0.));
#2723=DIRECTION('ref_axis',(1.,0.,0.));
#2724=DIRECTION('',(1.,0.,0.));
#2725=DIRECTION('',(1.,0.,0.));
#2726=DIRECTION('',(0.,0.,1.));
#2727=DIRECTION('center_axis',(-1.,0.,0.));
#2728=DIRECTION('ref_axis',(0.,-1.,0.));
#2729=DIRECTION('',(0.,-1.,0.));
#2730=DIRECTION('',(0.,-1.,0.));
#2731=DIRECTION('center_axis',(0.,0.,1.));
#2732=DIRECTION('ref_axis',(1.,0.,0.));
#2733=DIRECTION('center_axis',(0.,0.,1.));
#2734=DIRECTION('ref_axis',(1.,0.,0.));
#2735=DIRECTION('axis',(0.,0.,1.));
#2736=DIRECTION('refdir',(1.,0.,0.));
#2737=DIRECTION('center_axis',(0.,1.,0.));
#2738=DIRECTION('ref_axis',(1.,0.,0.));
#2739=DIRECTION('center_axis',(0.,1.,0.));
#2740=DIRECTION('ref_axis',(1.,0.,0.));
#2741=DIRECTION('',(0.,1.,0.));
#2742=DIRECTION('center_axis',(0.,1.,0.));
#2743=DIRECTION('ref_axis',(1.,0.,0.));
#2744=DIRECTION('center_axis',(0.,1.,0.));
#2745=DIRECTION('ref_axis',(1.,0.,0.));
#2746=DIRECTION('center_axis',(0.,1.,0.));
#2747=DIRECTION('ref_axis',(1.,0.,0.));
#2748=DIRECTION('center_axis',(0.,1.,0.));
#2749=DIRECTION('ref_axis',(1.,0.,0.));
#2750=DIRECTION('',(0.,1.,0.));
#2751=DIRECTION('',(0.,1.,0.));
#2752=DIRECTION('center_axis',(0.,1.,0.));
#2753=DIRECTION('ref_axis',(1.,0.,0.));
#2754=DIRECTION('center_axis',(0.,1.,0.));
#2755=DIRECTION('ref_axis',(1.,0.,0.));
#2756=DIRECTION('center_axis',(1.,0.,0.));
#2757=DIRECTION('ref_axis',(0.,0.,-1.));
#2758=DIRECTION('center_axis',(1.,0.,0.));
#2759=DIRECTION('ref_axis',(0.,0.,-1.));
#2760=DIRECTION('',(1.,0.,0.));
#2761=DIRECTION('center_axis',(1.,0.,0.));
#2762=DIRECTION('ref_axis',(0.,0.,-1.));
#2763=DIRECTION('center_axis',(1.,0.,0.));
#2764=DIRECTION('ref_axis',(0.,0.,-1.));
#2765=DIRECTION('',(1.,0.,0.));
#2766=DIRECTION('center_axis',(1.,0.,0.));
#2767=DIRECTION('ref_axis',(0.,0.,-1.));
#2768=DIRECTION('center_axis',(1.,0.,0.));
#2769=DIRECTION('ref_axis',(0.,0.,-1.));
#2770=DIRECTION('center_axis',(0.,1.,0.));
#2771=DIRECTION('ref_axis',(-1.,0.,0.));
#2772=DIRECTION('',(-1.,0.,0.));
#2773=DIRECTION('',(0.,0.,1.));
#2774=DIRECTION('',(-1.,0.,0.));
#2775=DIRECTION('',(0.,0.,1.));
#2776=DIRECTION('center_axis',(1.,0.,0.));
#2777=DIRECTION('ref_axis',(0.,1.,0.));
#2778=DIRECTION('',(0.,1.,0.));
#2779=DIRECTION('',(0.,1.,0.));
#2780=DIRECTION('',(0.,0.,1.));
#2781=DIRECTION('center_axis',(0.,-1.,0.));
#2782=DIRECTION('ref_axis',(1.,0.,0.));
#2783=DIRECTION('',(1.,0.,0.));
#2784=DIRECTION('',(1.,0.,0.));
#2785=DIRECTION('',(0.,0.,1.));
#2786=DIRECTION('center_axis',(-1.,0.,0.));
#2787=DIRECTION('ref_axis',(0.,-1.,0.));
#2788=DIRECTION('',(0.,-1.,0.));
#2789=DIRECTION('',(0.,-1.,0.));
#2790=DIRECTION('center_axis',(0.,0.,1.));
#2791=DIRECTION('ref_axis',(1.,0.,0.));
#2792=DIRECTION('center_axis',(0.,0.,1.));
#2793=DIRECTION('ref_axis',(1.,0.,0.));
#2794=DIRECTION('axis',(0.,0.,1.));
#2795=DIRECTION('refdir',(1.,0.,0.));
#2796=DIRECTION('center_axis',(1.,0.,0.));
#2797=DIRECTION('ref_axis',(0.,0.,-1.));
#2798=DIRECTION('',(0.,0.,1.));
#2799=DIRECTION('center_axis',(1.,0.,0.));
#2800=DIRECTION('ref_axis',(0.,0.,-1.));
#2801=DIRECTION('',(0.,0.,-1.));
#2802=DIRECTION('',(0.,-1.,0.));
#2803=DIRECTION('center_axis',(1.,0.,0.));
#2804=DIRECTION('ref_axis',(0.,0.,-1.));
#2805=DIRECTION('',(1.,0.,0.));
#2806=DIRECTION('',(1.,0.,0.));
#2807=DIRECTION('center_axis',(1.,0.,0.));
#2808=DIRECTION('ref_axis',(0.,0.,-1.));
#2809=DIRECTION('',(-1.,0.,0.));
#2810=DIRECTION('',(-1.,0.,0.));
#2811=DIRECTION('center_axis',(0.,0.,1.));
#2812=DIRECTION('ref_axis',(1.,0.,0.));
#2813=DIRECTION('',(0.,0.,-1.));
#2814=DIRECTION('center_axis',(0.,0.,1.));
#2815=DIRECTION('ref_axis',(1.,0.,0.));
#2816=DIRECTION('',(0.,0.,1.));
#2817=DIRECTION('center_axis',(0.,0.,1.));
#2818=DIRECTION('ref_axis',(1.,0.,0.));
#2819=DIRECTION('',(0.,0.,1.));
#2820=DIRECTION('center_axis',(0.,0.,-1.));
#2821=DIRECTION('ref_axis',(1.,0.,0.));
#2822=DIRECTION('center_axis',(0.,0.,-1.));
#2823=DIRECTION('ref_axis',(1.,0.,0.));
#2824=DIRECTION('center_axis',(0.,0.,1.));
#2825=DIRECTION('ref_axis',(1.,0.,0.));
#2826=DIRECTION('center_axis',(0.,0.,1.));
#2827=DIRECTION('ref_axis',(1.,0.,0.));
#2828=DIRECTION('center_axis',(0.,0.,1.));
#2829=DIRECTION('ref_axis',(1.,0.,0.));
#2830=DIRECTION('',(0.,0.,1.));
#2831=DIRECTION('center_axis',(0.,0.,-1.));
#2832=DIRECTION('ref_axis',(1.,0.,0.));
#2833=DIRECTION('center_axis',(0.,0.,-1.));
#2834=DIRECTION('ref_axis',(1.,0.,0.));
#2835=DIRECTION('center_axis',(0.,0.,1.));
#2836=DIRECTION('ref_axis',(1.,0.,0.));
#2837=DIRECTION('center_axis',(0.,0.,1.));
#2838=DIRECTION('ref_axis',(1.,0.,0.));
#2839=DIRECTION('',(0.,0.,1.));
#2840=DIRECTION('center_axis',(0.,0.,-1.));
#2841=DIRECTION('ref_axis',(1.,0.,0.));
#2842=DIRECTION('center_axis',(0.,0.,-1.));
#2843=DIRECTION('ref_axis',(1.,0.,0.));
#2844=DIRECTION('center_axis',(0.,0.,1.));
#2845=DIRECTION('ref_axis',(1.,0.,0.));
#2846=DIRECTION('',(0.,0.,-1.));
#2847=DIRECTION('center_axis',(0.,0.,1.));
#2848=DIRECTION('ref_axis',(1.,0.,0.));
#2849=DIRECTION('',(0.,0.,1.));
#2850=DIRECTION('center_axis',(0.,0.,-1.));
#2851=DIRECTION('ref_axis',(1.,0.,0.));
#2852=DIRECTION('center_axis',(0.,0.,1.));
#2853=DIRECTION('ref_axis',(1.,0.,0.));
#2854=DIRECTION('',(0.,0.,1.));
#2855=DIRECTION('center_axis',(0.,0.,1.));
#2856=DIRECTION('ref_axis',(1.,0.,0.));
#2857=DIRECTION('center_axis',(1.,0.,0.));
#2858=DIRECTION('ref_axis',(0.,0.,-1.));
#2859=DIRECTION('',(0.,1.,0.));
#2860=DIRECTION('',(0.,0.,1.));
#2861=DIRECTION('',(0.,1.,0.));
#2862=DIRECTION('center_axis',(0.,0.,1.));
#2863=DIRECTION('ref_axis',(1.,0.,0.));
#2864=DIRECTION('',(0.,1.,0.));
#2865=DIRECTION('',(-1.,0.,0.));
#2866=DIRECTION('',(0.,-1.,0.));
#2867=DIRECTION('',(0.,-1.,0.));
#2868=DIRECTION('center_axis',(0.,0.,1.));
#2869=DIRECTION('ref_axis',(1.,0.,0.));
#2870=DIRECTION('center_axis',(0.,0.,1.));
#2871=DIRECTION('ref_axis',(1.,0.,0.));
#2872=DIRECTION('',(0.,-1.,0.));
#2873=DIRECTION('',(1.,0.,0.));
#2874=DIRECTION('',(0.,1.,0.));
#2875=DIRECTION('center_axis',(0.,0.,1.));
#2876=DIRECTION('ref_axis',(1.,0.,0.));
#2877=DIRECTION('center_axis',(0.,0.,1.));
#2878=DIRECTION('ref_axis',(1.,0.,0.));
#2879=DIRECTION('center_axis',(0.,0.,1.));
#2880=DIRECTION('ref_axis',(1.,0.,0.));
#2881=DIRECTION('center_axis',(0.,0.,-1.));
#2882=DIRECTION('ref_axis',(1.,0.,0.));
#2883=DIRECTION('center_axis',(0.,0.,-1.));
#2884=DIRECTION('ref_axis',(1.,0.,0.));
#2885=DIRECTION('center_axis',(0.,0.,1.));
#2886=DIRECTION('ref_axis',(1.,0.,0.));
#2887=DIRECTION('center_axis',(0.,0.,1.));
#2888=DIRECTION('ref_axis',(1.,0.,0.));
#2889=DIRECTION('',(0.,0.,1.));
#2890=DIRECTION('center_axis',(0.,0.,1.));
#2891=DIRECTION('ref_axis',(1.,0.,0.));
#2892=DIRECTION('center_axis',(0.,0.,1.));
#2893=DIRECTION('ref_axis',(1.,0.,0.));
#2894=DIRECTION('center_axis',(0.,0.,1.));
#2895=DIRECTION('ref_axis',(1.,0.,0.));
#2896=DIRECTION('',(0.,1.,0.));
#2897=DIRECTION('',(1.,0.,0.));
#2898=DIRECTION('',(0.,-1.,0.));
#2899=DIRECTION('center_axis',(0.,0.,1.));
#2900=DIRECTION('ref_axis',(1.,0.,0.));
#2901=DIRECTION('',(0.,-1.,0.));
#2902=DIRECTION('',(0.,-1.,0.));
#2903=DIRECTION('',(-1.,0.,0.));
#2904=DIRECTION('',(0.,1.,0.));
#2905=DIRECTION('center_axis',(0.,0.,1.));
#2906=DIRECTION('ref_axis',(1.,0.,0.));
#2907=DIRECTION('center_axis',(0.,0.,1.));
#2908=DIRECTION('ref_axis',(1.,0.,0.));
#2909=DIRECTION('center_axis',(0.,0.,1.));
#2910=DIRECTION('ref_axis',(1.,0.,0.));
#2911=DIRECTION('',(0.,0.,-1.));
#2912=DIRECTION('',(0.,0.,1.));
#2913=DIRECTION('center_axis',(0.,0.,-1.));
#2914=DIRECTION('ref_axis',(1.,0.,0.));
#2915=DIRECTION('center_axis',(1.,0.,0.));
#2916=DIRECTION('ref_axis',(0.,0.,-1.));
#2917=DIRECTION('',(0.,0.,-1.));
#2918=DIRECTION('center_axis',(0.,0.,1.));
#2919=DIRECTION('ref_axis',(1.,0.,0.));
#2920=DIRECTION('center_axis',(0.,0.,1.));
#2921=DIRECTION('ref_axis',(1.,0.,0.));
#2922=DIRECTION('',(0.,0.,1.));
#2923=DIRECTION('center_axis',(1.,0.,0.));
#2924=DIRECTION('ref_axis',(0.,0.,-1.));
#2925=DIRECTION('',(0.,0.,1.));
#2926=DIRECTION('center_axis',(1.,0.,0.));
#2927=DIRECTION('ref_axis',(0.,0.,-1.));
#2928=DIRECTION('',(0.,0.,1.));
#2929=DIRECTION('center_axis',(0.,0.,1.));
#2930=DIRECTION('ref_axis',(1.,0.,0.));
#2931=DIRECTION('center_axis',(0.,0.,1.));
#2932=DIRECTION('ref_axis',(1.,0.,0.));
#2933=DIRECTION('',(0.,0.,1.));
#2934=DIRECTION('center_axis',(1.,0.,0.));
#2935=DIRECTION('ref_axis',(0.,0.,-1.));
#2936=DIRECTION('',(0.,0.,-1.));
#2937=DIRECTION('center_axis',(0.,0.,1.));
#2938=DIRECTION('ref_axis',(1.,0.,0.));
#2939=DIRECTION('',(0.,0.,1.));
#2940=DIRECTION('',(0.,0.,1.));
#2941=DIRECTION('center_axis',(0.,0.,-1.));
#2942=DIRECTION('ref_axis',(1.,0.,0.));
#2943=DIRECTION('center_axis',(0.,0.,-1.));
#2944=DIRECTION('ref_axis',(1.,0.,0.));
#2945=DIRECTION('center_axis',(0.,0.,1.));
#2946=DIRECTION('ref_axis',(1.,0.,0.));
#2947=DIRECTION('center_axis',(0.,0.,1.));
#2948=DIRECTION('ref_axis',(1.,0.,0.));
#2949=DIRECTION('',(0.,0.,1.));
#2950=DIRECTION('center_axis',(1.,0.,0.));
#2951=DIRECTION('ref_axis',(0.,0.,-1.));
#2952=DIRECTION('',(0.,0.,-1.));
#2953=DIRECTION('center_axis',(0.,0.,1.));
#2954=DIRECTION('ref_axis',(1.,0.,0.));
#2955=DIRECTION('',(0.,0.,1.));
#2956=DIRECTION('center_axis',(0.,0.,-1.));
#2957=DIRECTION('ref_axis',(1.,0.,0.));
#2958=DIRECTION('center_axis',(0.,0.,1.));
#2959=DIRECTION('ref_axis',(1.,0.,0.));
#2960=DIRECTION('',(0.,0.,1.));
#2961=DIRECTION('center_axis',(0.,0.,-1.));
#2962=DIRECTION('ref_axis',(1.,0.,0.));
#2963=DIRECTION('center_axis',(1.,0.,0.));
#2964=DIRECTION('ref_axis',(0.,1.,0.));
#2965=DIRECTION('',(0.,0.,1.));
#2966=DIRECTION('',(0.,1.,0.));
#2967=DIRECTION('',(0.,0.,1.));
#2968=DIRECTION('',(0.,-1.,0.));
#2969=DIRECTION('center_axis',(0.,-1.,0.));
#2970=DIRECTION('ref_axis',(1.,0.,0.));
#2971=DIRECTION('',(1.,0.,0.));
#2972=DIRECTION('',(0.,0.,1.));
#2973=DIRECTION('',(1.,0.,0.));
#2974=DIRECTION('center_axis',(0.,0.,1.));
#2975=DIRECTION('ref_axis',(0.,-1.,0.));
#2976=DIRECTION('',(0.,-1.,0.));
#2977=DIRECTION('',(1.,0.,0.));
#2978=DIRECTION('',(0.,-1.,0.));
#2979=DIRECTION('center_axis',(0.,1.,0.));
#2980=DIRECTION('ref_axis',(-1.,0.,0.));
#2981=DIRECTION('',(-1.,0.,0.));
#2982=DIRECTION('',(0.,0.,1.));
#2983=DIRECTION('center_axis',(-1.,0.,0.));
#2984=DIRECTION('ref_axis',(0.,-1.,0.));
#2985=DIRECTION('',(0.,-1.,0.));
#2986=DIRECTION('center_axis',(0.,0.,1.));
#2987=DIRECTION('ref_axis',(1.,0.,0.));
#2988=DIRECTION('axis',(0.,0.,1.));
#2989=DIRECTION('refdir',(1.,0.,0.));
#2990=DIRECTION('center_axis',(0.,1.,0.));
#2991=DIRECTION('ref_axis',(1.,0.,0.));
#2992=DIRECTION('',(-0.5,0.,0.866025403784439));
#2993=DIRECTION('',(-1.,0.,-2.84883360945713E-16));
#2994=DIRECTION('',(-0.5,0.,-0.866025403784439));
#2995=DIRECTION('',(0.5,0.,-0.866025403784439));
#2996=DIRECTION('',(1.,0.,0.));
#2997=DIRECTION('',(0.5,0.,0.866025403784439));
#2998=DIRECTION('center_axis',(0.,-1.,0.));
#2999=DIRECTION('ref_axis',(1.,0.,0.));
#3000=DIRECTION('center_axis',(0.,1.,0.));
#3001=DIRECTION('ref_axis',(1.,0.,0.));
#3002=DIRECTION('',(0.5,0.,-0.866025403784439));
#3003=DIRECTION('',(-0.5,0.,-0.866025403784439));
#3004=DIRECTION('',(-1.,0.,0.));
#3005=DIRECTION('',(-0.5,0.,0.866025403784439));
#3006=DIRECTION('',(0.5,0.,0.866025403784439));
#3007=DIRECTION('',(1.,0.,2.84883360945713E-16));
#3008=DIRECTION('center_axis',(0.,1.,0.));
#3009=DIRECTION('ref_axis',(1.,0.,0.));
#3010=DIRECTION('center_axis',(-2.84883360945713E-16,0.,1.));
#3011=DIRECTION('ref_axis',(1.,0.,2.84883360945713E-16));
#3012=DIRECTION('',(0.,-1.,0.));
#3013=DIRECTION('',(0.,1.,0.));
#3014=DIRECTION('center_axis',(-0.866025403784439,0.,0.5));
#3015=DIRECTION('ref_axis',(0.5,0.,0.866025403784439));
#3016=DIRECTION('',(0.,1.,0.));
#3017=DIRECTION('center_axis',(-0.866025403784439,0.,-0.5));
#3018=DIRECTION('ref_axis',(-0.5,0.,0.866025403784439));
#3019=DIRECTION('',(0.,1.,0.));
#3020=DIRECTION('center_axis',(0.,0.,-1.));
#3021=DIRECTION('ref_axis',(-1.,0.,0.));
#3022=DIRECTION('',(0.,1.,0.));
#3023=DIRECTION('center_axis',(0.866025403784439,0.,-0.5));
#3024=DIRECTION('ref_axis',(-0.5,0.,-0.866025403784439));
#3025=DIRECTION('',(0.,1.,0.));
#3026=DIRECTION('center_axis',(0.866025403784439,0.,0.5));
#3027=DIRECTION('ref_axis',(0.5,0.,-0.866025403784439));
#3028=DIRECTION('center_axis',(0.,-1.,0.));
#3029=DIRECTION('ref_axis',(1.,0.,0.));
#3030=DIRECTION('',(0.,1.,0.));
#3031=DIRECTION('center_axis',(0.,-1.,0.));
#3032=DIRECTION('ref_axis',(1.,0.,0.));
#3033=DIRECTION('center_axis',(0.,1.,0.));
#3034=DIRECTION('ref_axis',(0.,0.,1.));
#3035=DIRECTION('center_axis',(0.,-1.,0.));
#3036=DIRECTION('ref_axis',(1.,0.,0.));
#3037=DIRECTION('center_axis',(0.,-1.,0.));
#3038=DIRECTION('ref_axis',(1.,0.,0.));
#3039=DIRECTION('center_axis',(0.,-1.,0.));
#3040=DIRECTION('ref_axis',(1.,0.,0.));
#3041=DIRECTION('',(0.707106781186547,0.707106781186548,8.65956056235493E-17));
#3042=DIRECTION('center_axis',(0.,-1.,0.));
#3043=DIRECTION('ref_axis',(1.,0.,0.));
#3044=DIRECTION('center_axis',(0.,-1.,0.));
#3045=DIRECTION('ref_axis',(1.,0.,0.));
#3046=DIRECTION('',(0.,1.,0.));
#3047=DIRECTION('center_axis',(0.,1.,0.));
#3048=DIRECTION('ref_axis',(1.,0.,0.));
#3049=DIRECTION('center_axis',(0.,-1.,0.));
#3050=DIRECTION('ref_axis',(1.,0.,0.));
#3051=DIRECTION('',(-0.707106781186547,0.707106781186548,-8.65956056235493E-17));
#3052=DIRECTION('center_axis',(0.,-1.,0.));
#3053=DIRECTION('ref_axis',(0.,0.,-1.));
#3054=DIRECTION('center_axis',(0.,-1.,0.));
#3055=DIRECTION('ref_axis',(1.,0.,0.));
#3056=DIRECTION('center_axis',(0.,-1.,0.));
#3057=DIRECTION('ref_axis',(1.,0.,0.));
#3058=DIRECTION('',(0.,1.,0.));
#3059=DIRECTION('axis',(0.,0.,1.));
#3060=DIRECTION('refdir',(1.,0.,0.));
#3061=DIRECTION('center_axis',(0.,0.,1.));
#3062=DIRECTION('ref_axis',(1.,0.,0.));
#3063=DIRECTION('center_axis',(0.,0.,1.));
#3064=DIRECTION('ref_axis',(1.,0.,0.));
#3065=DIRECTION('',(0.707106781186549,8.65956056235495E-17,-0.707106781186546));
#3066=DIRECTION('center_axis',(0.,0.,1.));
#3067=DIRECTION('ref_axis',(1.,0.,0.));
#3068=DIRECTION('center_axis',(0.,0.,1.));
#3069=DIRECTION('ref_axis',(1.,0.,0.));
#3070=DIRECTION('',(0.316227766016837,3.87267321454038E-17,-0.948683298050514));
#3071=DIRECTION('center_axis',(0.,0.,1.));
#3072=DIRECTION('ref_axis',(1.,0.,0.));
#3073=DIRECTION('center_axis',(0.,0.,1.));
#3074=DIRECTION('ref_axis',(1.,0.,0.));
#3075=DIRECTION('',(0.,0.,-1.));
#3076=DIRECTION('center_axis',(0.,0.,-1.));
#3077=DIRECTION('ref_axis',(-1.,0.,0.));
#3078=DIRECTION('center_axis',(0.,0.,1.));
#3079=DIRECTION('ref_axis',(1.,0.,0.));
#3080=DIRECTION('center_axis',(0.,0.,1.));
#3081=DIRECTION('ref_axis',(1.,0.,0.));
#3082=DIRECTION('center_axis',(0.,0.,1.));
#3083=DIRECTION('ref_axis',(1.,0.,0.));
#3084=DIRECTION('',(0.,0.,-1.));
#3085=DIRECTION('center_axis',(0.,0.,1.));
#3086=DIRECTION('ref_axis',(1.,0.,0.));
#3087=DIRECTION('axis',(0.,0.,1.));
#3088=DIRECTION('refdir',(1.,0.,0.));
#3089=DIRECTION('center_axis',(0.,-1.,0.));
#3090=DIRECTION('ref_axis',(0.,0.,-1.));
#3091=DIRECTION('center_axis',(-1.,0.,-1.22464679914735E-16));
#3092=DIRECTION('ref_axis',(-1.22464679914735E-16,0.,1.));
#3093=DIRECTION('center_axis',(0.,1.,0.));
#3094=DIRECTION('ref_axis',(0.,0.,-1.));
#3095=DIRECTION('axis',(0.,0.,1.));
#3096=DIRECTION('refdir',(1.,0.,0.));
#3097=DIRECTION('center_axis',(0.,1.,0.));
#3098=DIRECTION('ref_axis',(1.,0.,0.));
#3099=DIRECTION('center_axis',(0.,1.,0.));
#3100=DIRECTION('ref_axis',(1.,0.,0.));
#3101=DIRECTION('center_axis',(0.,1.,0.));
#3102=DIRECTION('ref_axis',(1.,0.,0.));
#3103=DIRECTION('center_axis',(0.,1.,0.));
#3104=DIRECTION('ref_axis',(1.,0.,0.));
#3105=DIRECTION('',(0.,-1.,0.));
#3106=DIRECTION('center_axis',(0.,1.,0.));
#3107=DIRECTION('ref_axis',(1.,0.,0.));
#3108=DIRECTION('center_axis',(0.,1.,0.));
#3109=DIRECTION('ref_axis',(1.,0.,0.));
#3110=DIRECTION('center_axis',(0.,1.,0.));
#3111=DIRECTION('ref_axis',(1.,0.,0.));
#3112=DIRECTION('center_axis',(0.,1.,0.));
#3113=DIRECTION('ref_axis',(1.,0.,0.));
#3114=DIRECTION('',(0.,-1.,0.));
#3115=DIRECTION('center_axis',(0.,1.,0.));
#3116=DIRECTION('ref_axis',(1.,0.,0.));
#3117=DIRECTION('center_axis',(0.,1.,0.));
#3118=DIRECTION('ref_axis',(1.,0.,0.));
#3119=DIRECTION('center_axis',(0.,1.,0.));
#3120=DIRECTION('ref_axis',(1.,0.,0.));
#3121=DIRECTION('',(0.,-1.,0.));
#3122=DIRECTION('center_axis',(0.,1.,0.));
#3123=DIRECTION('ref_axis',(1.,0.,0.));
#3124=DIRECTION('center_axis',(0.,1.,0.));
#3125=DIRECTION('ref_axis',(1.,0.,0.));
#3126=DIRECTION('center_axis',(0.,1.,0.));
#3127=DIRECTION('ref_axis',(1.,0.,0.));
#3128=DIRECTION('center_axis',(-1.,0.,0.));
#3129=DIRECTION('ref_axis',(0.,0.,1.));
#3130=DIRECTION('',(0.,0.,-1.));
#3131=DIRECTION('',(0.,1.,0.));
#3132=DIRECTION('',(0.,0.,1.));
#3133=DIRECTION('',(0.,1.,0.));
#3134=DIRECTION('center_axis',(0.,0.,-1.));
#3135=DIRECTION('ref_axis',(-1.,0.,0.));
#3136=DIRECTION('',(1.,0.,0.));
#3137=DIRECTION('',(-1.,0.,0.));
#3138=DIRECTION('',(0.,1.,0.));
#3139=DIRECTION('center_axis',(1.,0.,0.));
#3140=DIRECTION('ref_axis',(0.,0.,-1.));
#3141=DIRECTION('',(0.,0.,1.));
#3142=DIRECTION('',(0.,0.,-1.));
#3143=DIRECTION('',(0.,1.,0.));
#3144=DIRECTION('center_axis',(0.986393923832144,0.,0.164398987305357));
#3145=DIRECTION('ref_axis',(0.164398987305357,0.,-0.986393923832144));
#3146=DIRECTION('',(-0.164398987305357,0.,0.986393923832144));
#3147=DIRECTION('',(0.164398987305357,0.,-0.986393923832144));
#3148=DIRECTION('',(0.,1.,0.));
#3149=DIRECTION('center_axis',(-0.986393923832144,0.,0.164398987305357));
#3150=DIRECTION('ref_axis',(0.164398987305357,0.,0.986393923832144));
#3151=DIRECTION('',(-0.164398987305357,0.,-0.986393923832144));
#3152=DIRECTION('',(0.164398987305357,0.,0.986393923832144));
#3153=DIRECTION('center_axis',(0.,1.,0.));
#3154=DIRECTION('ref_axis',(0.,0.,1.));
#3155=DIRECTION('center_axis',(0.,1.,0.));
#3156=DIRECTION('ref_axis',(1.,0.,0.));
#3157=DIRECTION('axis',(0.,0.,1.));
#3158=DIRECTION('refdir',(1.,0.,0.));
#3159=DIRECTION('center_axis',(0.,-1.,0.));
#3160=DIRECTION('ref_axis',(1.,0.,0.));
#3161=DIRECTION('center_axis',(0.,1.,0.));
#3162=DIRECTION('ref_axis',(1.,0.,0.));
#3163=DIRECTION('',(0.,1.,0.));
#3164=DIRECTION('center_axis',(0.,-1.,0.));
#3165=DIRECTION('ref_axis',(1.,0.,0.));
#3166=DIRECTION('center_axis',(0.,1.,0.));
#3167=DIRECTION('ref_axis',(1.,0.,0.));
#3168=DIRECTION('center_axis',(0.,-1.,0.));
#3169=DIRECTION('ref_axis',(1.,0.,0.));
#3170=DIRECTION('',(-0.707106781186547,0.707106781186548,-8.65956056235493E-17));
#3171=DIRECTION('center_axis',(0.,-1.,0.));
#3172=DIRECTION('ref_axis',(0.,0.,-1.));
#3173=DIRECTION('center_axis',(0.,-1.,0.));
#3174=DIRECTION('ref_axis',(1.,0.,0.));
#3175=DIRECTION('center_axis',(0.,1.,0.));
#3176=DIRECTION('ref_axis',(1.,0.,0.));
#3177=DIRECTION('',(-0.866025403784439,-0.5,-1.06057523872491E-16));
#3178=DIRECTION('center_axis',(1.92296268638356E-16,0.,-1.));
#3179=DIRECTION('ref_axis',(-1.,0.,-1.92296268638356E-16));
#3180=DIRECTION('',(0.,1.,0.));
#3181=DIRECTION('',(-1.,0.,-1.92296268638356E-16));
#3182=DIRECTION('',(0.,1.,0.));
#3183=DIRECTION('center_axis',(0.866025403784439,0.,-0.5));
#3184=DIRECTION('ref_axis',(-0.5,0.,-0.866025403784439));
#3185=DIRECTION('',(0.,1.,0.));
#3186=DIRECTION('',(-0.5,0.,-0.866025403784439));
#3187=DIRECTION('center_axis',(0.866025403784439,0.,0.5));
#3188=DIRECTION('ref_axis',(0.5,0.,-0.866025403784439));
#3189=DIRECTION('',(0.,1.,0.));
#3190=DIRECTION('',(0.5,0.,-0.866025403784439));
#3191=DIRECTION('center_axis',(-1.92296268638356E-16,0.,1.));
#3192=DIRECTION('ref_axis',(1.,0.,1.92296268638356E-16));
#3193=DIRECTION('',(0.,1.,0.));
#3194=DIRECTION('',(1.,0.,1.92296268638356E-16));
#3195=DIRECTION('center_axis',(-0.866025403784439,0.,0.5));
#3196=DIRECTION('ref_axis',(0.5,0.,0.866025403784439));
#3197=DIRECTION('',(0.,1.,0.));
#3198=DIRECTION('',(0.5,0.,0.866025403784439));
#3199=DIRECTION('center_axis',(-0.866025403784439,0.,-0.5));
#3200=DIRECTION('ref_axis',(-0.5,0.,0.866025403784439));
#3201=DIRECTION('',(-0.5,0.,0.866025403784438));
#3202=DIRECTION('center_axis',(0.,1.,0.));
#3203=DIRECTION('ref_axis',(0.,0.,1.));
#3204=DIRECTION('center_axis',(0.,1.,0.));
#3205=DIRECTION('ref_axis',(1.,0.,0.));
#3206=DIRECTION('',(0.,0.,1.));
#3207=DIRECTION('',(1.,0.,0.));
#3208=DIRECTION('',(0.,0.,1.));
#3209=DIRECTION('',(1.,0.,0.));
#3210=DIRECTION('',(0.,0.,1.));
#3211=DIRECTION('',(1.,0.,0.));
#3212=DIRECTION('',(0.,0.,1.));
#3213=DIRECTION('',(2.22044604925031E-16,-1.,0.));
#3214=DIRECTION('',(0.,0.,1.));
#3215=DIRECTION('',(2.22044604925031E-16,-1.,0.));
#3216=DIRECTION('',(0.,0.,1.));
#3217=DIRECTION('',(1.,0.,0.));
#3218=DIRECTION('',(0.,-1.,2.22044604925031E-16));
#3219=DIRECTION('',(1.,0.,0.));
#3220=DIRECTION('',(0.,0.,1.));
#3221=DIRECTION('',(1.,0.,0.));
#3222=DIRECTION('',(0.,1.,2.22044604925031E-16));
#3223=DIRECTION('',(1.,0.,0.));
#3224=DIRECTION('',(0.,1.,2.22044604925031E-16));
#3225=DIRECTION('',(1.,0.,0.));
#3226=DIRECTION('',(0.,1.,2.22044604925031E-16));
#3227=DIRECTION('',(1.,0.,0.));
#3228=DIRECTION('',(0.,1.,2.22044604925031E-16));
#3229=DIRECTION('',(1.,0.,0.));
#3230=DIRECTION('',(0.,0.,1.));
#3231=DIRECTION('',(1.,0.,0.));
#3232=CARTESIAN_POINT('',(0.,0.,0.));
#3233=CARTESIAN_POINT('',(0.,0.,0.));
#3234=CARTESIAN_POINT('',(0.,0.,0.));
#3235=CARTESIAN_POINT('Origin',(0.,0.,8.2));
#3236=CARTESIAN_POINT('',(-0.4,-4.89858719658941E-17,8.2));
#3237=CARTESIAN_POINT('',(-0.4,-4.89858719658941E-17,8.9));
#3238=CARTESIAN_POINT('',(-0.4,-4.89858719658941E-17,8.2));
#3239=CARTESIAN_POINT('',(0.299999999999998,0.264575131106461,8.2));
#3240=CARTESIAN_POINT('Origin',(0.,0.,8.2));
#3241=CARTESIAN_POINT('',(0.,0.4,8.5));
#3242=CARTESIAN_POINT('Origin',(0.,0.,8.5));
#3243=CARTESIAN_POINT('',(0.4,0.,8.9));
#3244=CARTESIAN_POINT('Origin',(0.,0.,8.5));
#3245=CARTESIAN_POINT('Origin',(0.,0.,8.9));
#3246=CARTESIAN_POINT('Origin',(1.5,1.4,4.9));
#3247=CARTESIAN_POINT('',(1.25,1.4,5.));
#3248=CARTESIAN_POINT('Origin',(1.5,1.4,5.));
#3249=CARTESIAN_POINT('',(1.25,1.4,7.3));
#3250=CARTESIAN_POINT('',(1.25,1.4,4.9));
#3251=CARTESIAN_POINT('Origin',(1.5,1.4,7.3));
#3252=CARTESIAN_POINT('Origin',(1.5,1.4,7.3));
#3253=CARTESIAN_POINT('Origin',(1.5,-1.4,4.9));
#3254=CARTESIAN_POINT('',(1.25,-1.4,5.));
#3255=CARTESIAN_POINT('Origin',(1.5,-1.4,5.));
#3256=CARTESIAN_POINT('',(1.25,-1.4,7.3));
#3257=CARTESIAN_POINT('',(1.25,-1.4,4.9));
#3258=CARTESIAN_POINT('Origin',(1.5,-1.4,7.3));
#3259=CARTESIAN_POINT('Origin',(1.5,-1.4,7.3));
#3260=CARTESIAN_POINT('Origin',(-1.5,1.4,4.9));
#3261=CARTESIAN_POINT('',(-1.75,1.4,5.));
#3262=CARTESIAN_POINT('Origin',(-1.5,1.4,5.));
#3263=CARTESIAN_POINT('',(-1.75,1.4,7.3));
#3264=CARTESIAN_POINT('',(-1.75,1.4,4.9));
#3265=CARTESIAN_POINT('Origin',(-1.5,1.4,7.3));
#3266=CARTESIAN_POINT('Origin',(-1.5,1.4,7.3));
#3267=CARTESIAN_POINT('Origin',(-1.5,-1.4,4.9));
#3268=CARTESIAN_POINT('',(-1.75,-1.4,5.));
#3269=CARTESIAN_POINT('Origin',(-1.5,-1.4,5.));
#3270=CARTESIAN_POINT('',(-1.75,-1.4,7.3));
#3271=CARTESIAN_POINT('',(-1.75,-1.4,4.9));
#3272=CARTESIAN_POINT('Origin',(-1.5,-1.4,7.3));
#3273=CARTESIAN_POINT('Origin',(-1.5,-1.4,7.3));
#3274=CARTESIAN_POINT('Origin',(0.,0.,8.5));
#3275=CARTESIAN_POINT('',(0.,-0.264575131106461,8.2));
#3276=CARTESIAN_POINT('',(0.,-0.2,8.2));
#3277=CARTESIAN_POINT('',(0.,0.,8.2));
#3278=CARTESIAN_POINT('',(0.,-0.2,8.15358983848622));
#3279=CARTESIAN_POINT('Origin',(0.,0.,8.5));
#3280=CARTESIAN_POINT('',(0.,-0.2,5.9));
#3281=CARTESIAN_POINT('Origin',(0.,0.,8.5));
#3282=CARTESIAN_POINT('',(0.,0.264575131106461,8.2));
#3283=CARTESIAN_POINT('',(0.,0.264575131106461,8.2));
#3284=CARTESIAN_POINT('',(0.,0.2,8.15358983848622));
#3285=CARTESIAN_POINT('Origin',(0.,0.,8.5));
#3286=CARTESIAN_POINT('Ctrl Pts',(-6.93889390390723E-18,-0.2,8.15358983848622));
#3287=CARTESIAN_POINT('Ctrl Pts',(0.0256610133920982,-0.2,8.15358983848622));
#3288=CARTESIAN_POINT('Ctrl Pts',(0.0526277202526568,-0.194777116895352,
8.15043491280941));
#3289=CARTESIAN_POINT('Ctrl Pts',(0.101716471901564,-0.174245741947245,
8.13976079750786));
#3290=CARTESIAN_POINT('Ctrl Pts',(0.123891546848412,-0.158951165626207,
8.13245990649023));
#3291=CARTESIAN_POINT('Ctrl Pts',(0.158903378513366,-0.123939333961253,
8.1192266779859));
#3292=CARTESIAN_POINT('Ctrl Pts',(0.174233015984916,-0.101748151622875,
8.1123470317921));
#3293=CARTESIAN_POINT('Ctrl Pts',(0.194792781173826,-0.0525890150977706,
8.10268160632987));
#3294=CARTESIAN_POINT('Ctrl Pts',(0.2,-0.0255910602217378,8.1));
#3295=CARTESIAN_POINT('Ctrl Pts',(0.2,0.0255910602217378,8.1));
#3296=CARTESIAN_POINT('Ctrl Pts',(0.194792781173826,0.0525890150977706,
8.10268160632987));
#3297=CARTESIAN_POINT('Ctrl Pts',(0.174233015984916,0.101748151622875,8.1123470317921));
#3298=CARTESIAN_POINT('Ctrl Pts',(0.158903378513366,0.123939333961253,8.1192266779859));
#3299=CARTESIAN_POINT('Ctrl Pts',(0.123891546848412,0.158951165626207,8.13245990649023));
#3300=CARTESIAN_POINT('Ctrl Pts',(0.101716471901564,0.174245741947245,8.13976079750786));
#3301=CARTESIAN_POINT('Ctrl Pts',(0.0526277202526568,0.194777116895352,
8.15043491280941));
#3302=CARTESIAN_POINT('Ctrl Pts',(0.0256610133920983,0.2,8.15358983848622));
#3303=CARTESIAN_POINT('Ctrl Pts',(2.08166817117217E-17,0.2,8.15358983848622));
#3304=CARTESIAN_POINT('',(0.299999999999998,-0.264575131106461,8.2));
#3305=CARTESIAN_POINT('',(0.,-0.264575131106461,8.2));
#3306=CARTESIAN_POINT('',(0.,-0.4,8.5));
#3307=CARTESIAN_POINT('Origin',(0.,0.,8.5));
#3308=CARTESIAN_POINT('Origin',(0.,0.,8.5));
#3309=CARTESIAN_POINT('',(1.2,4.89858719658942E-17,8.9));
#3310=CARTESIAN_POINT('',(0.,-4.89858719658942E-17,8.9));
#3311=CARTESIAN_POINT('Origin',(1.2,0.,8.5));
#3312=CARTESIAN_POINT('Origin',(0.,0.,8.5));
#3313=CARTESIAN_POINT('',(0.,0.2,8.2));
#3314=CARTESIAN_POINT('',(0.,0.,8.2));
#3315=CARTESIAN_POINT('',(0.,0.2,5.9));
#3316=CARTESIAN_POINT('Origin',(1.2,0.,8.5));
#3317=CARTESIAN_POINT('',(1.2,-1.13892152320704E-16,9.43));
#3318=CARTESIAN_POINT('Origin',(1.2,0.,8.5));
#3319=CARTESIAN_POINT('',(2.5,1.13892152320704E-16,9.43));
#3320=CARTESIAN_POINT('',(1.2,-1.13892152320704E-16,9.43));
#3321=CARTESIAN_POINT('Origin',(2.5,0.,8.5));
#3322=CARTESIAN_POINT('Origin',(1.2,0.,8.5));
#3323=CARTESIAN_POINT('Origin',(0.,0.,9.7));
#3324=CARTESIAN_POINT('',(-0.49,-6.00076931582203E-17,9.7));
#3325=CARTESIAN_POINT('Origin',(0.,0.,9.7));
#3326=CARTESIAN_POINT('',(-0.49,-6.00076931582203E-17,9.9));
#3327=CARTESIAN_POINT('',(-0.49,-6.00076931582203E-17,9.7));
#3328=CARTESIAN_POINT('Origin',(0.,0.,9.9));
#3329=CARTESIAN_POINT('Origin',(0.,0.,9.9));
#3330=CARTESIAN_POINT('',(-0.25,3.06161699786838E-17,9.9));
#3331=CARTESIAN_POINT('Origin',(0.,0.,9.9));
#3332=CARTESIAN_POINT('Origin',(0.,0.,9.7));
#3333=CARTESIAN_POINT('',(-0.25,-3.06161699786838E-17,9.7));
#3334=CARTESIAN_POINT('Origin',(0.,0.,9.7));
#3335=CARTESIAN_POINT('Origin',(0.,0.,8.8));
#3336=CARTESIAN_POINT('',(-0.25,-3.06161699786838E-17,8.9));
#3337=CARTESIAN_POINT('Origin',(0.,0.,8.9));
#3338=CARTESIAN_POINT('',(-0.25,-3.06161699786838E-17,8.8));
#3339=CARTESIAN_POINT('Origin',(0.,0.,8.8));
#3340=CARTESIAN_POINT('',(-0.25,3.06161699786838E-17,10.));
#3341=CARTESIAN_POINT('',(-0.25,-3.06161699786838E-17,8.8));
#3342=CARTESIAN_POINT('Origin',(0.,0.,10.));
#3343=CARTESIAN_POINT('Origin',(0.,0.,8.2));
#3344=CARTESIAN_POINT('Origin',(0.,0.,8.9));
#3345=CARTESIAN_POINT('Origin',(0.,0.,8.2));
#3346=CARTESIAN_POINT('Origin',(0.,0.,8.9));
#3347=CARTESIAN_POINT('Origin',(0.,0.,8.2));
#3348=CARTESIAN_POINT('',(-0.2,-2.44929359829471E-17,8.2));
#3349=CARTESIAN_POINT('Origin',(0.,0.,8.2));
#3350=CARTESIAN_POINT('Origin',(0.,0.,8.2));
#3351=CARTESIAN_POINT('Origin',(0.,0.,5.9));
#3352=CARTESIAN_POINT('',(0.1,-0.173205080756888,5.9));
#3353=CARTESIAN_POINT('',(0.1,0.173205080756888,5.9));
#3354=CARTESIAN_POINT('',(0.1,0.,5.9));
#3355=CARTESIAN_POINT('Origin',(0.,0.,5.9));
#3356=CARTESIAN_POINT('Origin',(0.,0.,5.9));
#3357=CARTESIAN_POINT('',(0.1,-0.173205080756888,6.77077882690172));
#3358=CARTESIAN_POINT('',(0.1,-0.173205080756888,5.9));
#3359=CARTESIAN_POINT('',(-0.2,-3.65325966551488E-17,6.79));
#3360=CARTESIAN_POINT('Ctrl Pts',(-0.2,-3.46944695195361E-17,6.79));
#3361=CARTESIAN_POINT('Ctrl Pts',(-0.2,-0.0252293032709816,6.79));
#3362=CARTESIAN_POINT('Ctrl Pts',(-0.194935517523083,-0.0520663682763995,
6.78867047644404));
#3363=CARTESIAN_POINT('Ctrl Pts',(-0.174490207856786,-0.101311053228714,
6.78386739800365));
#3364=CARTESIAN_POINT('Ctrl Pts',(-0.159115319800683,-0.123727392673936,
6.78045818190283));
#3365=CARTESIAN_POINT('Ctrl Pts',(-0.123724786645461,-0.159117925829158,
6.77401874806683));
#3366=CARTESIAN_POINT('Ctrl Pts',(-0.101309531057858,-0.174490782742294,
6.77056050717812));
#3367=CARTESIAN_POINT('Ctrl Pts',(-0.0520686947820295,-0.19493460869448,
6.76564419277622));
#3368=CARTESIAN_POINT('Ctrl Pts',(-0.0252330191304887,-0.2,6.76426435217142));
#3369=CARTESIAN_POINT('Ctrl Pts',(0.,-0.2,6.76426435217142));
#3370=CARTESIAN_POINT('Ctrl Pts',(0.0252330191304888,-0.2,6.76426435217142));
#3371=CARTESIAN_POINT('Ctrl Pts',(0.0520686947820297,-0.19493460869448,
6.76564419277622));
#3372=CARTESIAN_POINT('Ctrl Pts',(0.0847159677793139,-0.181380103583493,
6.76890376898488));
#3373=CARTESIAN_POINT('Ctrl Pts',(0.0925218917477068,-0.177522568569378,
6.7698086253353));
#3374=CARTESIAN_POINT('Ctrl Pts',(0.1,-0.173205080756888,6.77077882690173));
#3375=CARTESIAN_POINT('',(-0.2,-2.44929359829471E-17,5.9));
#3376=CARTESIAN_POINT('',(0.1,0.173205080756888,6.77077882690172));
#3377=CARTESIAN_POINT('Ctrl Pts',(0.1,0.173205080756888,6.77077882690173));
#3378=CARTESIAN_POINT('Ctrl Pts',(0.0925218917477067,0.177522568569378,
6.7698086253353));
#3379=CARTESIAN_POINT('Ctrl Pts',(0.0847159677793139,0.181380103583493,
6.76890376898488));
#3380=CARTESIAN_POINT('Ctrl Pts',(0.0520686947820296,0.19493460869448,6.76564419277622));
#3381=CARTESIAN_POINT('Ctrl Pts',(0.0252330191304888,0.2,6.76426435217142));
#3382=CARTESIAN_POINT('Ctrl Pts',(-0.0252330191304888,0.2,6.76426435217142));
#3383=CARTESIAN_POINT('Ctrl Pts',(-0.0520686947820297,0.19493460869448,
6.76564419277622));
#3384=CARTESIAN_POINT('Ctrl Pts',(-0.101309531057858,0.174490782742294,
6.77056050717812));
#3385=CARTESIAN_POINT('Ctrl Pts',(-0.123724786645461,0.159117925829158,
6.77401874806683));
#3386=CARTESIAN_POINT('Ctrl Pts',(-0.159115319800683,0.123727392673936,
6.78045818190283));
#3387=CARTESIAN_POINT('Ctrl Pts',(-0.174490207856786,0.101311053228714,
6.78386739800365));
#3388=CARTESIAN_POINT('Ctrl Pts',(-0.194935517523083,0.0520663682763994,
6.78867047644404));
#3389=CARTESIAN_POINT('Ctrl Pts',(-0.2,0.0252293032709816,6.79));
#3390=CARTESIAN_POINT('Ctrl Pts',(-0.2,-6.24500451351651E-17,6.79));
#3391=CARTESIAN_POINT('',(0.1,0.173205080756888,5.9));
#3392=CARTESIAN_POINT('Origin',(0.1,0.,6.));
#3393=CARTESIAN_POINT('Origin',(0.1,0.,6.));
#3394=CARTESIAN_POINT('Origin',(-1.3,0.,6.));
#3395=CARTESIAN_POINT('',(-1.2,-9.67470971326409E-17,6.79));
#3396=CARTESIAN_POINT('Origin',(-1.2,0.,6.));
#3397=CARTESIAN_POINT('',(-1.3,-9.67470971326409E-17,6.79));
#3398=CARTESIAN_POINT('Origin',(-2.6,0.,6.));
#3399=CARTESIAN_POINT('',(-2.5,-1.13892152320704E-16,6.93));
#3400=CARTESIAN_POINT('Origin',(-2.5,0.,6.));
#3401=CARTESIAN_POINT('',(-1.2,-1.13892152320704E-16,6.93));
#3402=CARTESIAN_POINT('',(-2.6,-1.13892152320704E-16,6.93));
#3403=CARTESIAN_POINT('Origin',(-1.2,0.,6.));
#3404=CARTESIAN_POINT('Origin',(-1.2,0.,6.));
#3405=CARTESIAN_POINT('Origin',(2.5,2.,5.));
#3406=CARTESIAN_POINT('',(2.5,2.,5.));
#3407=CARTESIAN_POINT('',(-2.5,2.,5.));
#3408=CARTESIAN_POINT('',(2.5,2.,5.));
#3409=CARTESIAN_POINT('',(-2.5,2.,10.));
#3410=CARTESIAN_POINT('',(-2.5,2.,5.));
#3411=CARTESIAN_POINT('',(2.5,2.,10.));
#3412=CARTESIAN_POINT('',(2.5,2.,10.));
#3413=CARTESIAN_POINT('',(2.5,2.,5.));
#3414=CARTESIAN_POINT('Origin',(2.5,-2.,5.));
#3415=CARTESIAN_POINT('',(2.5,-2.,5.));
#3416=CARTESIAN_POINT('',(2.5,-2.,5.));
#3417=CARTESIAN_POINT('',(2.5,-2.,10.));
#3418=CARTESIAN_POINT('',(2.5,-2.,10.));
#3419=CARTESIAN_POINT('',(2.5,-2.,5.));
#3420=CARTESIAN_POINT('Origin',(-2.5,-2.,5.));
#3421=CARTESIAN_POINT('',(-2.5,-2.,5.));
#3422=CARTESIAN_POINT('',(-2.5,-2.,5.));
#3423=CARTESIAN_POINT('',(-2.5,-2.,10.));
#3424=CARTESIAN_POINT('',(-2.5,-2.,10.));
#3425=CARTESIAN_POINT('',(-2.5,-2.,5.));
#3426=CARTESIAN_POINT('Origin',(-2.5,2.,5.));
#3427=CARTESIAN_POINT('',(-2.5,2.,5.));
#3428=CARTESIAN_POINT('',(-2.5,2.,10.));
#3429=CARTESIAN_POINT('Origin',(0.,0.,10.));
#3430=CARTESIAN_POINT('Origin',(0.,0.,5.));
#3431=CARTESIAN_POINT('',(0.,0.,0.));
#3432=CARTESIAN_POINT('Origin',(8.,0.,8.5));
#3433=CARTESIAN_POINT('',(7.8,0.1,8.5));
#3434=CARTESIAN_POINT('Origin',(8.,0.1,8.5));
#3435=CARTESIAN_POINT('',(7.8,0.4,8.5));
#3436=CARTESIAN_POINT('',(7.8,0.,8.5));
#3437=CARTESIAN_POINT('Origin',(8.,0.4,8.5));
#3438=CARTESIAN_POINT('Origin',(8.,0.4,8.5));
#3439=CARTESIAN_POINT('Origin',(8.,-1.6,8.5));
#3440=CARTESIAN_POINT('',(7.315,-1.5,8.5));
#3441=CARTESIAN_POINT('Origin',(8.,-1.5,8.5));
#3442=CARTESIAN_POINT('',(7.315,-0.0250000000000004,8.5));
#3443=CARTESIAN_POINT('',(7.315,-1.6,8.5));
#3444=CARTESIAN_POINT('',(7.31545635639501,-3.06161699786843E-18,8.525));
#3445=CARTESIAN_POINT('Ctrl Pts',(7.31545635639501,6.50521303742584E-19,
8.525));
#3446=CARTESIAN_POINT('Ctrl Pts',(7.31545635639501,-0.00313935488643177,
8.525));
#3447=CARTESIAN_POINT('Ctrl Pts',(7.31543253912522,-0.00648777233356316,
8.5243725421486));
#3448=CARTESIAN_POINT('Ctrl Pts',(7.31534646113093,-0.0126471731738094,
8.521821113914));
#3449=CARTESIAN_POINT('Ctrl Pts',(7.31528543721954,-0.0154581801568198,
8.51989715890251));
#3450=CARTESIAN_POINT('Ctrl Pts',(7.31517084314585,-0.0198971587695597,
8.51545818028977));
#3451=CARTESIAN_POINT('Ctrl Pts',(7.31510983697032,-0.0218211138748799,
8.51264717324355));
#3452=CARTESIAN_POINT('Ctrl Pts',(7.31502379952475,-0.0243725422072981,
8.50648777221657));
#3453=CARTESIAN_POINT('Ctrl Pts',(7.315,-0.0250000000000004,8.50313935469838));
#3454=CARTESIAN_POINT('Ctrl Pts',(7.315,-0.0250000000000004,8.5));
#3455=CARTESIAN_POINT('',(7.315,0.0250000000000004,8.5));
#3456=CARTESIAN_POINT('Ctrl Pts',(7.315,0.0250000000000004,8.5));
#3457=CARTESIAN_POINT('Ctrl Pts',(7.315,0.0250000000000004,8.50313935469838));
#3458=CARTESIAN_POINT('Ctrl Pts',(7.31502379952475,0.0243725422072981,8.50648777221657));
#3459=CARTESIAN_POINT('Ctrl Pts',(7.31510983697032,0.0218211138748799,8.51264717324355));
#3460=CARTESIAN_POINT('Ctrl Pts',(7.31517084314585,0.0198971587695597,8.51545818028977));
#3461=CARTESIAN_POINT('Ctrl Pts',(7.31528543721954,0.0154581801568198,8.51989715890251));
#3462=CARTESIAN_POINT('Ctrl Pts',(7.31534646113093,0.0126471731738094,8.521821113914));
#3463=CARTESIAN_POINT('Ctrl Pts',(7.31543253912522,0.00648777233356315,
8.5243725421486));
#3464=CARTESIAN_POINT('Ctrl Pts',(7.31545635639501,0.00313935488643177,
8.525));
#3465=CARTESIAN_POINT('Ctrl Pts',(7.31545635639501,6.50521303491303E-19,
8.525));
#3466=CARTESIAN_POINT('',(7.315,0.1,8.5));
#3467=CARTESIAN_POINT('',(7.315,-1.6,8.5));
#3468=CARTESIAN_POINT('Origin',(8.,0.1,8.5));
#3469=CARTESIAN_POINT('',(7.31545635639501,0.,8.475));
#3470=CARTESIAN_POINT('Ctrl Pts',(7.31545635639501,0.,8.475));
#3471=CARTESIAN_POINT('Ctrl Pts',(7.31545635639501,0.00313935488643177,
8.475));
#3472=CARTESIAN_POINT('Ctrl Pts',(7.31543253912522,0.00648777233356316,
8.4756274578514));
#3473=CARTESIAN_POINT('Ctrl Pts',(7.31534646113093,0.0126471731738094,8.478178886086));
#3474=CARTESIAN_POINT('Ctrl Pts',(7.31528543721954,0.0154581801568198,8.48010284109749));
#3475=CARTESIAN_POINT('Ctrl Pts',(7.31517084314585,0.0198971587695597,8.48454181971023));
#3476=CARTESIAN_POINT('Ctrl Pts',(7.31510983697032,0.0218211138748799,8.48735282675645));
#3477=CARTESIAN_POINT('Ctrl Pts',(7.31502379952475,0.0243725422072981,8.49351222778343));
#3478=CARTESIAN_POINT('Ctrl Pts',(7.315,0.0250000000000004,8.49686064530162));
#3479=CARTESIAN_POINT('Ctrl Pts',(7.315,0.0250000000000004,8.5));
#3480=CARTESIAN_POINT('Ctrl Pts',(7.315,-0.0250000000000004,8.5));
#3481=CARTESIAN_POINT('Ctrl Pts',(7.315,-0.0250000000000004,8.49686064530162));
#3482=CARTESIAN_POINT('Ctrl Pts',(7.31502379952475,-0.0243725422072981,
8.49351222778343));
#3483=CARTESIAN_POINT('Ctrl Pts',(7.31510983697032,-0.0218211138748799,
8.48735282675645));
#3484=CARTESIAN_POINT('Ctrl Pts',(7.31517084314585,-0.0198971587695597,
8.48454181971023));
#3485=CARTESIAN_POINT('Ctrl Pts',(7.31528543721954,-0.0154581801568198,
8.48010284109749));
#3486=CARTESIAN_POINT('Ctrl Pts',(7.31534646113093,-0.012647173173808,8.478178886086));
#3487=CARTESIAN_POINT('Ctrl Pts',(7.31543253912522,-0.00648777233356145,
8.4756274578514));
#3488=CARTESIAN_POINT('Ctrl Pts',(7.31545635639501,-0.00313935488643176,
8.475));
#3489=CARTESIAN_POINT('Ctrl Pts',(7.31545635639501,0.,8.475));
#3490=CARTESIAN_POINT('Origin',(8.,0.1,8.5));
#3491=CARTESIAN_POINT('Origin',(7.2,0.,8.5));
#3492=CARTESIAN_POINT('',(7.3,-3.06161699786843E-18,8.525));
#3493=CARTESIAN_POINT('Origin',(7.3,0.,8.5));
#3494=CARTESIAN_POINT('',(7.2,-3.06161699786843E-18,8.525));
#3495=CARTESIAN_POINT('Origin',(5.9,0.,8.5));
#3496=CARTESIAN_POINT('',(6.,-1.13892152320704E-16,9.43));
#3497=CARTESIAN_POINT('Origin',(6.,0.,8.5));
#3498=CARTESIAN_POINT('',(7.3,-1.13892152320704E-16,9.43));
#3499=CARTESIAN_POINT('',(5.9,-1.13892152320704E-16,9.43));
#3500=CARTESIAN_POINT('Origin',(7.3,0.,8.5));
#3501=CARTESIAN_POINT('Origin',(7.3,0.,8.5));
#3502=CARTESIAN_POINT('Origin',(9.,1.5,7.));
#3503=CARTESIAN_POINT('',(9.,1.5,7.));
#3504=CARTESIAN_POINT('',(6.,1.5,7.));
#3505=CARTESIAN_POINT('',(9.,1.5,7.));
#3506=CARTESIAN_POINT('',(6.,1.5,10.));
#3507=CARTESIAN_POINT('',(6.,1.5,7.));
#3508=CARTESIAN_POINT('',(9.,1.5,10.));
#3509=CARTESIAN_POINT('',(9.,1.5,10.));
#3510=CARTESIAN_POINT('',(9.,1.5,7.));
#3511=CARTESIAN_POINT('Origin',(9.,-1.5,7.));
#3512=CARTESIAN_POINT('',(9.,-1.5,7.));
#3513=CARTESIAN_POINT('',(9.,-1.5,7.));
#3514=CARTESIAN_POINT('',(9.,-1.5,10.));
#3515=CARTESIAN_POINT('',(9.,-1.5,10.));
#3516=CARTESIAN_POINT('',(9.,-1.5,7.));
#3517=CARTESIAN_POINT('Origin',(6.,-1.5,7.));
#3518=CARTESIAN_POINT('',(6.,-1.5,7.));
#3519=CARTESIAN_POINT('',(6.,-1.5,7.));
#3520=CARTESIAN_POINT('',(6.,-1.5,10.));
#3521=CARTESIAN_POINT('',(6.,-1.5,10.));
#3522=CARTESIAN_POINT('',(6.,-1.5,7.));
#3523=CARTESIAN_POINT('Origin',(6.,1.5,7.));
#3524=CARTESIAN_POINT('',(6.,1.5,7.));
#3525=CARTESIAN_POINT('',(6.,1.5,10.));
#3526=CARTESIAN_POINT('Origin',(7.5,0.,10.));
#3527=CARTESIAN_POINT('Origin',(7.5,0.,7.));
#3528=CARTESIAN_POINT('',(0.,0.,0.));
#3529=CARTESIAN_POINT('Origin',(-1.2,0.,6.));
#3530=CARTESIAN_POINT('',(-1.2,1.26252272915133,4.86156407366234));
#3531=CARTESIAN_POINT('',(-1.2,1.26252272915133,5.));
#3532=CARTESIAN_POINT('',(-1.2,1.26252272915133,4.1));
#3533=CARTESIAN_POINT('',(-1.2,-1.26252272915133,4.86156407366234));
#3534=CARTESIAN_POINT('Origin',(-1.2,0.,6.));
#3535=CARTESIAN_POINT('',(-1.2,-1.26252272915133,5.));
#3536=CARTESIAN_POINT('',(-1.2,-1.26252272915133,4.1));
#3537=CARTESIAN_POINT('',(-1.2,1.25,5.));
#3538=CARTESIAN_POINT('Origin',(-3.6,0.,6.));
#3539=CARTESIAN_POINT('',(-1.82903432003806,1.37477270848678,5.));
#3540=CARTESIAN_POINT('Ctrl Pts',(-1.82903432003806,1.37477270848676,5.00000000000002));
#3541=CARTESIAN_POINT('Ctrl Pts',(-1.82812531946363,1.36291680291864,4.98370082459056));
#3542=CARTESIAN_POINT('Ctrl Pts',(-1.82653488263586,1.35063671201868,4.96743485680573));
#3543=CARTESIAN_POINT('Ctrl Pts',(-1.81822884513887,1.30711001024898,4.91188459887471));
#3544=CARTESIAN_POINT('Ctrl Pts',(-1.80714205446995,1.27468449144834,4.87434693316054));
#3545=CARTESIAN_POINT('Ctrl Pts',(-1.77578652436294,1.21580790152752,4.81103672837552));
#3546=CARTESIAN_POINT('Ctrl Pts',(-1.75030832988751,1.18152448377587,4.77719694611154));
#3547=CARTESIAN_POINT('Ctrl Pts',(-1.69569663875101,1.13196676018157,4.73126383714339));
#3548=CARTESIAN_POINT('Ctrl Pts',(-1.66179162252479,1.10939592163522,4.71172525423958));
#3549=CARTESIAN_POINT('Ctrl Pts',(-1.5846841815694,1.07835439237347,4.6856321341911));
#3550=CARTESIAN_POINT('Ctrl Pts',(-1.54146883053287,1.07,4.67897766862176));
#3551=CARTESIAN_POINT('Ctrl Pts',(-1.45853116946713,1.07,4.67897766862176));
#3552=CARTESIAN_POINT('Ctrl Pts',(-1.4153158184306,1.07835439237347,4.6856321341911));
#3553=CARTESIAN_POINT('Ctrl Pts',(-1.33820837747521,1.10939592163522,4.71172525423958));
#3554=CARTESIAN_POINT('Ctrl Pts',(-1.30430336124899,1.13196676018157,4.73126383714339));
#3555=CARTESIAN_POINT('Ctrl Pts',(-1.24969167011249,1.18152448377587,4.77719694611154));
#3556=CARTESIAN_POINT('Ctrl Pts',(-1.22421347563706,1.21580790152752,4.81103672837552));
#3557=CARTESIAN_POINT('Ctrl Pts',(-1.20564651189243,1.25067127353037,4.84852543524467));
#3558=CARTESIAN_POINT('Ctrl Pts',(-1.20273149014269,1.25656212898995,4.85495378228886));
#3559=CARTESIAN_POINT('Ctrl Pts',(-1.2,1.26252272915133,4.86156407366234));
#3560=CARTESIAN_POINT('',(-2.4511708863178,1.37477270848675,5.));
#3561=CARTESIAN_POINT('',(-3.6,1.37477270848675,5.));
#3562=CARTESIAN_POINT('',(-3.1488291136822,1.37477270848675,5.));
#3563=CARTESIAN_POINT('Ctrl Pts',(-3.1488291136822,1.37477270848675,5.));
#3564=CARTESIAN_POINT('Ctrl Pts',(-3.11342817786855,1.34573205820429,4.96007570655496));
#3565=CARTESIAN_POINT('Ctrl Pts',(-3.06914962012721,1.31716857379013,4.92472362043486));
#3566=CARTESIAN_POINT('Ctrl Pts',(-2.98559269661871,1.28103353525338,4.88222090056834));
#3567=CARTESIAN_POINT('Ctrl Pts',(-2.95013776503027,1.26954894147296,4.86934551918671));
#3568=CARTESIAN_POINT('Ctrl Pts',(-2.87639593827315,1.25402991358996,4.85215722115304));
#3569=CARTESIAN_POINT('Ctrl Pts',(-2.83811186099248,1.25,4.84782813781971));
#3570=CARTESIAN_POINT('Ctrl Pts',(-2.76188813900752,1.25,4.84782813781971));
#3571=CARTESIAN_POINT('Ctrl Pts',(-2.72360406172685,1.25402991358996,4.85215722115304));
#3572=CARTESIAN_POINT('Ctrl Pts',(-2.64986223496973,1.26954894147297,4.86934551918671));
#3573=CARTESIAN_POINT('Ctrl Pts',(-2.61440730338129,1.28103353525338,4.88222090056834));
#3574=CARTESIAN_POINT('Ctrl Pts',(-2.53085037987278,1.31716857379013,4.92472362043486));
#3575=CARTESIAN_POINT('Ctrl Pts',(-2.48657182213145,1.34573205820429,4.96007570655496));
#3576=CARTESIAN_POINT('Ctrl Pts',(-2.4511708863178,1.37477270848675,5.));
#3577=CARTESIAN_POINT('',(-3.5,1.37477270848675,5.));
#3578=CARTESIAN_POINT('',(-3.6,1.37477270848675,5.));
#3579=CARTESIAN_POINT('',(-3.5,-1.37477270848675,5.));
#3580=CARTESIAN_POINT('Origin',(-3.5,0.,6.));
#3581=CARTESIAN_POINT('',(-3.1488291136822,-1.37477270848675,5.));
#3582=CARTESIAN_POINT('',(-3.6,-1.37477270848675,5.));
#3583=CARTESIAN_POINT('',(-2.4511708863178,-1.37477270848675,5.));
#3584=CARTESIAN_POINT('Ctrl Pts',(-2.4511708863178,-1.37477270848675,5.));
#3585=CARTESIAN_POINT('Ctrl Pts',(-2.48657182213145,-1.34573205820429,4.96007570655496));
#3586=CARTESIAN_POINT('Ctrl Pts',(-2.53085037987278,-1.31716857379013,4.92472362043486));
#3587=CARTESIAN_POINT('Ctrl Pts',(-2.61440730338129,-1.28103353525338,4.88222090056834));
#3588=CARTESIAN_POINT('Ctrl Pts',(-2.64986223496973,-1.26954894147297,4.86934551918671));
#3589=CARTESIAN_POINT('Ctrl Pts',(-2.72360406172685,-1.25402991358996,4.85215722115304));
#3590=CARTESIAN_POINT('Ctrl Pts',(-2.76188813900752,-1.25,4.84782813781971));
#3591=CARTESIAN_POINT('Ctrl Pts',(-2.8,-1.25,4.84782813781971));
#3592=CARTESIAN_POINT('Ctrl Pts',(-2.83811186099248,-1.25,4.84782813781971));
#3593=CARTESIAN_POINT('Ctrl Pts',(-2.87639593827315,-1.25402991358996,4.85215722115304));
#3594=CARTESIAN_POINT('Ctrl Pts',(-2.95013776503027,-1.26954894147297,4.86934551918671));
#3595=CARTESIAN_POINT('Ctrl Pts',(-2.98559269661871,-1.28103353525338,4.88222090056834));
#3596=CARTESIAN_POINT('Ctrl Pts',(-3.06914962012721,-1.31716857379013,4.92472362043486));
#3597=CARTESIAN_POINT('Ctrl Pts',(-3.11342817786855,-1.34573205820429,4.96007570655496));
#3598=CARTESIAN_POINT('Ctrl Pts',(-3.1488291136822,-1.37477270848675,5.));
#3599=CARTESIAN_POINT('',(-1.82903432003806,-1.37477270848678,5.));
#3600=CARTESIAN_POINT('',(-3.6,-1.37477270848675,5.));
#3601=CARTESIAN_POINT('Ctrl Pts',(-1.2,-1.26252272915133,4.86156407366234));
#3602=CARTESIAN_POINT('Ctrl Pts',(-1.20273149013951,-1.25656212899688,4.85495378229655));
#3603=CARTESIAN_POINT('Ctrl Pts',(-1.20564651188764,-1.25067127353937,4.84852543525435));
#3604=CARTESIAN_POINT('Ctrl Pts',(-1.22421347563706,-1.21580790152752,4.81103672837552));
#3605=CARTESIAN_POINT('Ctrl Pts',(-1.24969167011249,-1.18152448377587,4.77719694611154));
#3606=CARTESIAN_POINT('Ctrl Pts',(-1.30430336124899,-1.13196676018157,4.73126383714339));
#3607=CARTESIAN_POINT('Ctrl Pts',(-1.33820837747521,-1.10939592163522,4.71172525423958));
#3608=CARTESIAN_POINT('Ctrl Pts',(-1.4153158184306,-1.07835439237347,4.68563213419111));
#3609=CARTESIAN_POINT('Ctrl Pts',(-1.45853116946713,-1.07,4.67897766862176));
#3610=CARTESIAN_POINT('Ctrl Pts',(-1.5,-1.07,4.67897766862176));
#3611=CARTESIAN_POINT('Ctrl Pts',(-1.54146883053287,-1.07,4.67897766862176));
#3612=CARTESIAN_POINT('Ctrl Pts',(-1.5846841815694,-1.07835439237347,4.68563213419111));
#3613=CARTESIAN_POINT('Ctrl Pts',(-1.66179162252479,-1.10939592163522,4.71172525423958));
#3614=CARTESIAN_POINT('Ctrl Pts',(-1.69569663875101,-1.13196676018157,4.73126383714339));
#3615=CARTESIAN_POINT('Ctrl Pts',(-1.75030832988751,-1.18152448377587,4.77719694611154));
#3616=CARTESIAN_POINT('Ctrl Pts',(-1.77578652436294,-1.21580790152752,4.81103672837552));
#3617=CARTESIAN_POINT('Ctrl Pts',(-1.80714205446995,-1.27468449144834,4.87434693316054));
#3618=CARTESIAN_POINT('Ctrl Pts',(-1.81822884513887,-1.30711001024898,4.91188459887471));
#3619=CARTESIAN_POINT('Ctrl Pts',(-1.82653488263586,-1.35063671201868,4.96743485680573));
#3620=CARTESIAN_POINT('Ctrl Pts',(-1.82812531946363,-1.36291680291864,4.98370082459056));
#3621=CARTESIAN_POINT('Ctrl Pts',(-1.82903432003806,-1.37477270848676,5.00000000000002));
#3622=CARTESIAN_POINT('Origin',(-2.8,1.8,0.8));
#3623=CARTESIAN_POINT('',(-2.5,2.26097722286464,4.2));
#3624=CARTESIAN_POINT('',(-2.5,2.26097722286464,0.8));
#3625=CARTESIAN_POINT('',(-2.5,2.26097722286464,0.8));
#3626=CARTESIAN_POINT('',(-2.5,1.33902277713536,4.2));
#3627=CARTESIAN_POINT('Origin',(-2.8,1.8,4.2));
#3628=CARTESIAN_POINT('',(-2.5,1.33902277713536,0.8));
#3629=CARTESIAN_POINT('',(-2.5,1.33902277713536,0.8));
#3630=CARTESIAN_POINT('',(-3.35,1.8,0.8));
#3631=CARTESIAN_POINT('Origin',(-2.8,1.8,0.8));
#3632=CARTESIAN_POINT('',(-3.35,1.8,5.));
#3633=CARTESIAN_POINT('',(-3.35,1.8,0.8));
#3634=CARTESIAN_POINT('Origin',(-2.8,1.8,5.));
#3635=CARTESIAN_POINT('Origin',(-2.8,1.8,5.));
#3636=CARTESIAN_POINT('Origin',(-2.8,1.8,0.8));
#3637=CARTESIAN_POINT('Origin',(-1.5,1.4,4.1));
#3638=CARTESIAN_POINT('',(-1.83,1.4,4.2));
#3639=CARTESIAN_POINT('Origin',(-1.5,1.4,4.2));
#3640=CARTESIAN_POINT('',(-1.83,1.4,5.00000000000002));
#3641=CARTESIAN_POINT('',(-1.83,1.4,4.1));
#3642=CARTESIAN_POINT('Origin',(-1.5,1.4,5.));
#3643=CARTESIAN_POINT('Origin',(-1.5,1.4,5.));
#3644=CARTESIAN_POINT('Origin',(-1.5,-1.4,4.1));
#3645=CARTESIAN_POINT('',(-1.83,-1.4,4.2));
#3646=CARTESIAN_POINT('Origin',(-1.5,-1.4,4.2));
#3647=CARTESIAN_POINT('',(-1.83,-1.4,5.00000000000002));
#3648=CARTESIAN_POINT('',(-1.83,-1.4,4.1));
#3649=CARTESIAN_POINT('Origin',(-1.5,-1.4,5.));
#3650=CARTESIAN_POINT('Origin',(-1.5,-1.4,5.));
#3651=CARTESIAN_POINT('Origin',(2.8,1.8,0.8));
#3652=CARTESIAN_POINT('',(2.5,1.33902277713536,4.2));
#3653=CARTESIAN_POINT('',(2.5,1.33902277713536,0.8));
#3654=CARTESIAN_POINT('',(2.5,1.33902277713536,0.8));
#3655=CARTESIAN_POINT('',(2.25,1.8,4.2));
#3656=CARTESIAN_POINT('Origin',(2.8,1.8,4.2));
#3657=CARTESIAN_POINT('',(2.25,1.8,5.));
#3658=CARTESIAN_POINT('',(2.25,1.8,0.8));
#3659=CARTESIAN_POINT('Origin',(2.8,1.8,5.));
#3660=CARTESIAN_POINT('',(2.5,2.26097722286464,4.2));
#3661=CARTESIAN_POINT('Origin',(2.8,1.8,4.2));
#3662=CARTESIAN_POINT('',(2.5,2.26097722286464,0.8));
#3663=CARTESIAN_POINT('',(2.5,2.26097722286464,0.8));
#3664=CARTESIAN_POINT('Origin',(2.8,1.8,0.8));
#3665=CARTESIAN_POINT('Origin',(2.5,0.,2.85));
#3666=CARTESIAN_POINT('',(2.5,-1.33902277713536,0.8));
#3667=CARTESIAN_POINT('',(2.5,0.,0.8));
#3668=CARTESIAN_POINT('',(2.5,-1.33902277713536,4.2));
#3669=CARTESIAN_POINT('',(2.5,-1.33902277713536,0.8));
#3670=CARTESIAN_POINT('',(2.5,0.,4.2));
#3671=CARTESIAN_POINT('Origin',(0.,0.,0.8));
#3672=CARTESIAN_POINT('',(2.5,2.5,0.8));
#3673=CARTESIAN_POINT('',(2.5,0.,0.8));
#3674=CARTESIAN_POINT('',(-2.5,2.5,0.8));
#3675=CARTESIAN_POINT('',(3.5,2.5,0.8));
#3676=CARTESIAN_POINT('',(-2.5,0.,0.8));
#3677=CARTESIAN_POINT('',(-2.5,-1.33902277713536,0.8));
#3678=CARTESIAN_POINT('',(-2.5,0.,0.8));
#3679=CARTESIAN_POINT('',(-3.35,-1.8,0.8));
#3680=CARTESIAN_POINT('Origin',(-2.8,-1.8,0.8));
#3681=CARTESIAN_POINT('',(-2.5,-2.26097722286464,0.8));
#3682=CARTESIAN_POINT('Origin',(-2.8,-1.8,0.8));
#3683=CARTESIAN_POINT('',(-2.5,-2.5,0.8));
#3684=CARTESIAN_POINT('',(-2.5,0.,0.8));
#3685=CARTESIAN_POINT('',(2.5,-2.5,0.8));
#3686=CARTESIAN_POINT('',(-3.5,-2.5,0.8));
#3687=CARTESIAN_POINT('',(2.5,-2.26097722286464,0.8));
#3688=CARTESIAN_POINT('',(2.5,0.,0.8));
#3689=CARTESIAN_POINT('Origin',(2.8,-1.8,0.8));
#3690=CARTESIAN_POINT('',(2.47,-1.8,0.8));
#3691=CARTESIAN_POINT('Origin',(2.8,-1.8,0.8));
#3692=CARTESIAN_POINT('',(-3.13,-1.8,0.8));
#3693=CARTESIAN_POINT('Origin',(-2.8,-1.8,0.8));
#3694=CARTESIAN_POINT('',(-3.13,1.8,0.8));
#3695=CARTESIAN_POINT('Origin',(-2.8,1.8,0.8));
#3696=CARTESIAN_POINT('',(2.47,1.8,0.8));
#3697=CARTESIAN_POINT('Origin',(2.8,1.8,0.8));
#3698=CARTESIAN_POINT('Origin',(2.8,1.8,-0.1));
#3699=CARTESIAN_POINT('',(2.47,1.8,0.));
#3700=CARTESIAN_POINT('Origin',(2.8,1.8,0.));
#3701=CARTESIAN_POINT('',(2.47,1.8,-0.1));
#3702=CARTESIAN_POINT('Origin',(0.,0.,4.2));
#3703=CARTESIAN_POINT('',(2.25,-1.8,4.2));
#3704=CARTESIAN_POINT('Origin',(2.8,-1.8,4.2));
#3705=CARTESIAN_POINT('',(2.5,-2.26097722286464,4.2));
#3706=CARTESIAN_POINT('Origin',(2.8,-1.8,4.2));
#3707=CARTESIAN_POINT('',(2.5,-2.5,4.2));
#3708=CARTESIAN_POINT('',(2.5,0.,4.2));
#3709=CARTESIAN_POINT('',(-2.5,-2.5,4.2));
#3710=CARTESIAN_POINT('',(-3.5,-2.5,4.2));
#3711=CARTESIAN_POINT('',(-2.5,-2.26097722286464,4.2));
#3712=CARTESIAN_POINT('',(-2.5,0.,4.2));
#3713=CARTESIAN_POINT('',(-2.5,-1.33902277713536,4.2));
#3714=CARTESIAN_POINT('Origin',(-2.8,-1.8,4.2));
#3715=CARTESIAN_POINT('',(-2.5,0.,4.2));
#3716=CARTESIAN_POINT('',(-2.5,2.5,4.2));
#3717=CARTESIAN_POINT('',(-2.5,0.,4.2));
#3718=CARTESIAN_POINT('',(2.5,2.5,4.2));
#3719=CARTESIAN_POINT('',(3.5,2.5,4.2));
#3720=CARTESIAN_POINT('',(2.5,0.,4.2));
#3721=CARTESIAN_POINT('',(1.17,-1.4,4.2));
#3722=CARTESIAN_POINT('Origin',(1.5,-1.4,4.2));
#3723=CARTESIAN_POINT('',(1.17,1.4,4.2));
#3724=CARTESIAN_POINT('Origin',(1.5,1.4,4.2));
#3725=CARTESIAN_POINT('Origin',(2.8,-1.8,0.8));
#3726=CARTESIAN_POINT('',(2.5,-2.26097722286464,0.8));
#3727=CARTESIAN_POINT('',(2.25,-1.8,5.));
#3728=CARTESIAN_POINT('',(2.25,-1.8,0.8));
#3729=CARTESIAN_POINT('Origin',(2.8,-1.8,5.));
#3730=CARTESIAN_POINT('Origin',(2.5,0.,2.85));
#3731=CARTESIAN_POINT('',(2.5,-2.5,5.));
#3732=CARTESIAN_POINT('Origin',(2.8,-1.8,-0.1));
#3733=CARTESIAN_POINT('',(2.47,-1.8,0.));
#3734=CARTESIAN_POINT('Origin',(2.8,-1.8,0.));
#3735=CARTESIAN_POINT('',(2.47,-1.8,-0.1));
#3736=CARTESIAN_POINT('Origin',(2.5,0.,2.85));
#3737=CARTESIAN_POINT('',(2.5,2.5,0.7));
#3738=CARTESIAN_POINT('Origin',(-2.5,0.,2.85));
#3739=CARTESIAN_POINT('',(-2.5,2.5,0.7));
#3740=CARTESIAN_POINT('Origin',(-2.8,1.8,-0.1));
#3741=CARTESIAN_POINT('',(-3.13,1.8,0.));
#3742=CARTESIAN_POINT('Origin',(-2.8,1.8,0.));
#3743=CARTESIAN_POINT('',(-3.13,1.8,-0.1));
#3744=CARTESIAN_POINT('Origin',(-2.5,0.,2.85));
#3745=CARTESIAN_POINT('',(-2.5,-1.33902277713536,0.8));
#3746=CARTESIAN_POINT('Origin',(-2.8,-1.8,0.8));
#3747=CARTESIAN_POINT('',(-2.5,-2.26097722286464,0.8));
#3748=CARTESIAN_POINT('',(-3.35,-1.8,5.));
#3749=CARTESIAN_POINT('',(-3.35,-1.8,0.8));
#3750=CARTESIAN_POINT('Origin',(-2.8,-1.8,5.));
#3751=CARTESIAN_POINT('Origin',(-2.8,-1.8,5.));
#3752=CARTESIAN_POINT('Origin',(-2.8,-1.8,-0.1));
#3753=CARTESIAN_POINT('',(-3.13,-1.8,0.));
#3754=CARTESIAN_POINT('Origin',(-2.8,-1.8,0.));
#3755=CARTESIAN_POINT('',(-3.13,-1.8,-0.1));
#3756=CARTESIAN_POINT('Origin',(-2.5,0.,2.85));
#3757=CARTESIAN_POINT('',(-2.5,-2.5,5.));
#3758=CARTESIAN_POINT('Origin',(1.5,1.4,4.1));
#3759=CARTESIAN_POINT('',(1.17,1.4,5.));
#3760=CARTESIAN_POINT('',(1.17,1.4,4.1));
#3761=CARTESIAN_POINT('Origin',(1.5,1.4,5.));
#3762=CARTESIAN_POINT('Origin',(1.5,-1.4,4.1));
#3763=CARTESIAN_POINT('',(1.17,-1.4,5.));
#3764=CARTESIAN_POINT('',(1.17,-1.4,4.1));
#3765=CARTESIAN_POINT('Origin',(1.5,-1.4,5.));
#3766=CARTESIAN_POINT('Origin',(3.5,-2.5,0.));
#3767=CARTESIAN_POINT('',(3.5,-2.5,0.));
#3768=CARTESIAN_POINT('',(3.5,-2.5,5.));
#3769=CARTESIAN_POINT('',(3.5,-2.5,0.));
#3770=CARTESIAN_POINT('',(3.5,2.5,0.));
#3771=CARTESIAN_POINT('',(3.5,-2.5,0.));
#3772=CARTESIAN_POINT('',(3.5,2.5,5.));
#3773=CARTESIAN_POINT('',(3.5,2.5,0.));
#3774=CARTESIAN_POINT('',(3.5,2.5,5.));
#3775=CARTESIAN_POINT('Origin',(-3.5,-2.5,0.));
#3776=CARTESIAN_POINT('',(-3.5,-2.5,5.));
#3777=CARTESIAN_POINT('',(-3.5,-2.5,5.));
#3778=CARTESIAN_POINT('',(-3.5,-2.5,0.));
#3779=CARTESIAN_POINT('',(-3.5,-2.5,0.));
#3780=CARTESIAN_POINT('',(-3.5,-2.5,0.));
#3781=CARTESIAN_POINT('Origin',(2.5,2.5,5.));
#3782=CARTESIAN_POINT('',(-3.5,2.5,5.));
#3783=CARTESIAN_POINT('',(-3.5,2.5,5.));
#3784=CARTESIAN_POINT('',(2.5,2.5,5.));
#3785=CARTESIAN_POINT('',(-3.5,2.5,5.));
#3786=CARTESIAN_POINT('Origin',(3.5,2.5,0.));
#3787=CARTESIAN_POINT('',(-3.5,2.5,0.));
#3788=CARTESIAN_POINT('',(3.5,2.5,0.));
#3789=CARTESIAN_POINT('',(-3.5,2.5,0.));
#3790=CARTESIAN_POINT('Origin',(-3.5,2.5,0.));
#3791=CARTESIAN_POINT('',(-3.5,2.5,0.));
#3792=CARTESIAN_POINT('Origin',(0.,0.,0.));
#3793=CARTESIAN_POINT('',(0.,0.,0.));
#3794=CARTESIAN_POINT('Origin',(0.,-0.6,0.));
#3795=CARTESIAN_POINT('',(1.55884572681199,-0.6,0.));
#3796=CARTESIAN_POINT('',(0.779422863405995,-0.6,1.35));
#3797=CARTESIAN_POINT('',(0.779422863405995,-0.6,1.35));
#3798=CARTESIAN_POINT('',(-0.779422863405996,-0.6,1.35));
#3799=CARTESIAN_POINT('',(-0.779422863405996,-0.6,1.35));
#3800=CARTESIAN_POINT('',(-1.55884572681199,-0.6,-1.90903542970483E-16));
#3801=CARTESIAN_POINT('',(-1.55884572681199,-0.6,-1.90903542970483E-16));
#3802=CARTESIAN_POINT('',(-0.779422863405995,-0.6,-1.35));
#3803=CARTESIAN_POINT('',(-0.779422863405995,-0.6,-1.35));
#3804=CARTESIAN_POINT('',(0.779422863405995,-0.6,-1.35));
#3805=CARTESIAN_POINT('',(0.779422863405995,-0.6,-1.35));
#3806=CARTESIAN_POINT('',(1.55884572681199,-0.6,0.));
#3807=CARTESIAN_POINT('',(-1.065,-0.6,-1.30424884109193E-16));
#3808=CARTESIAN_POINT('Origin',(0.,-0.6,0.));
#3809=CARTESIAN_POINT('Origin',(0.,0.6,0.));
#3810=CARTESIAN_POINT('',(0.779422863405995,0.6,1.35));
#3811=CARTESIAN_POINT('',(1.55884572681199,0.6,0.));
#3812=CARTESIAN_POINT('',(0.779422863405995,0.6,1.35));
#3813=CARTESIAN_POINT('',(0.779422863405995,0.6,-1.35));
#3814=CARTESIAN_POINT('',(1.55884572681199,0.6,0.));
#3815=CARTESIAN_POINT('',(-0.779422863405995,0.6,-1.35));
#3816=CARTESIAN_POINT('',(0.779422863405995,0.6,-1.35));
#3817=CARTESIAN_POINT('',(-1.55884572681199,0.6,-1.90903542970483E-16));
#3818=CARTESIAN_POINT('',(-0.779422863405995,0.6,-1.35));
#3819=CARTESIAN_POINT('',(-0.779422863405996,0.6,1.35));
#3820=CARTESIAN_POINT('',(-1.55884572681199,0.6,-1.90903542970483E-16));
#3821=CARTESIAN_POINT('',(-0.779422863405996,0.6,1.35));
#3822=CARTESIAN_POINT('',(-1.065,0.6,1.30424884109193E-16));
#3823=CARTESIAN_POINT('Origin',(0.,0.6,0.));
#3824=CARTESIAN_POINT('Origin',(-0.779422863405996,0.,1.35));
#3825=CARTESIAN_POINT('',(0.779422863405995,0.,1.35));
#3826=CARTESIAN_POINT('',(-0.779422863405996,0.,1.35));
#3827=CARTESIAN_POINT('Origin',(-1.55884572681199,0.,-1.90903542970483E-16));
#3828=CARTESIAN_POINT('',(-1.55884572681199,0.,-1.90903542970483E-16));
#3829=CARTESIAN_POINT('Origin',(-0.779422863405995,0.,-1.35));
#3830=CARTESIAN_POINT('',(-0.779422863405995,0.,-1.35));
#3831=CARTESIAN_POINT('Origin',(0.779422863405995,0.,-1.35));
#3832=CARTESIAN_POINT('',(0.779422863405995,0.,-1.35));
#3833=CARTESIAN_POINT('Origin',(1.55884572681199,0.,0.));
#3834=CARTESIAN_POINT('',(1.55884572681199,0.,0.));
#3835=CARTESIAN_POINT('Origin',(0.779422863405995,0.,1.35));
#3836=CARTESIAN_POINT('Origin',(0.,0.,0.));
#3837=CARTESIAN_POINT('',(-1.065,2.47,-1.30424884109193E-16));
#3838=CARTESIAN_POINT('',(-1.065,0.,-1.30424884109193E-16));
#3839=CARTESIAN_POINT('Origin',(0.,2.47,0.));
#3840=CARTESIAN_POINT('Origin',(0.985,2.55,0.));
#3841=CARTESIAN_POINT('',(-0.985,2.55,-1.20627709716014E-16));
#3842=CARTESIAN_POINT('Origin',(0.,2.55,0.));
#3843=CARTESIAN_POINT('',(-0.79,2.55,-9.67470971326409E-17));
#3844=CARTESIAN_POINT('Origin',(0.,2.55,0.));
#3845=CARTESIAN_POINT('Origin',(0.,2.51,0.));
#3846=CARTESIAN_POINT('',(-1.025,2.51,-1.25526296912604E-16));
#3847=CARTESIAN_POINT('Origin',(0.,0.,0.));
#3848=CARTESIAN_POINT('',(-1.065,-2.47,-1.30424884109193E-16));
#3849=CARTESIAN_POINT('Origin',(0.,-2.47,0.));
#3850=CARTESIAN_POINT('',(-1.065,0.,-1.30424884109193E-16));
#3851=CARTESIAN_POINT('Origin',(0.,-2.51,0.));
#3852=CARTESIAN_POINT('',(-0.985,-2.55,-1.20627709716014E-16));
#3853=CARTESIAN_POINT('Origin',(0.,-2.55,0.));
#3854=CARTESIAN_POINT('',(-1.025,-2.51,-1.25526296912604E-16));
#3855=CARTESIAN_POINT('Origin',(0.79,-2.55,0.));
#3856=CARTESIAN_POINT('',(-0.79,-2.55,-9.67470971326409E-17));
#3857=CARTESIAN_POINT('Origin',(0.,-2.55,0.));
#3858=CARTESIAN_POINT('Origin',(0.,0.,0.));
#3859=CARTESIAN_POINT('',(-0.79,0.,-9.67470971326409E-17));
#3860=CARTESIAN_POINT('',(0.,0.,0.));
#3861=CARTESIAN_POINT('Origin',(0.,0.8,8.15));
#3862=CARTESIAN_POINT('',(-0.2,0.8,8.25));
#3863=CARTESIAN_POINT('Origin',(0.,0.8,8.25));
#3864=CARTESIAN_POINT('',(0.,0.8,8.05));
#3865=CARTESIAN_POINT('',(-0.1,0.8,8.15));
#3866=CARTESIAN_POINT('Origin',(0.,0.8,8.4));
#3867=CARTESIAN_POINT('',(-0.3,0.8,8.55));
#3868=CARTESIAN_POINT('Origin',(0.,0.8,8.55));
#3869=CARTESIAN_POINT('',(-0.25,0.8,8.4));
#3870=CARTESIAN_POINT('Origin',(0.,0.8,9.425));
#3871=CARTESIAN_POINT('',(-0.3,0.8,10.3));
#3872=CARTESIAN_POINT('Origin',(0.,0.8,10.3));
#3873=CARTESIAN_POINT('',(-0.3,0.8,9.425));
#3874=CARTESIAN_POINT('Origin',(0.6,0.8,10.3));
#3875=CARTESIAN_POINT('',(-0.6,0.8,10.3));
#3876=CARTESIAN_POINT('Origin',(0.,0.8,10.3));
#3877=CARTESIAN_POINT('Origin',(0.,0.8,10.6));
#3878=CARTESIAN_POINT('',(-0.6,0.8,10.9));
#3879=CARTESIAN_POINT('Origin',(0.,0.8,10.9));
#3880=CARTESIAN_POINT('',(-0.6,0.8,10.6));
#3881=CARTESIAN_POINT('Origin',(0.,0.8,10.9));
#3882=CARTESIAN_POINT('',(0.,0.,0.));
#3883=CARTESIAN_POINT('Origin',(0.,0.,0.));
#3884=CARTESIAN_POINT('',(-3.71680303541222E-17,-1.08993565124114E-17,0.3035));
#3885=CARTESIAN_POINT('Origin',(-4.80673868665336E-17,0.,0.3925));
#3886=CARTESIAN_POINT('Origin',(0.,1.08993565124114E-17,0.));
#3887=CARTESIAN_POINT('',(0.,0.,0.));
#3888=CARTESIAN_POINT('Origin',(0.,-5.2,2.9));
#3889=CARTESIAN_POINT('',(-2.,-5.2,2.9));
#3890=CARTESIAN_POINT('Origin',(0.,-5.2,2.9));
#3891=CARTESIAN_POINT('',(-0.685,-5.2,2.9));
#3892=CARTESIAN_POINT('Origin',(0.,-5.2,2.9));
#3893=CARTESIAN_POINT('Origin',(0.,-6.5,2.9));
#3894=CARTESIAN_POINT('',(-2.,-6.5,2.9));
#3895=CARTESIAN_POINT('',(-2.,-6.5,2.9));
#3896=CARTESIAN_POINT('Origin',(0.,-6.5,2.9));
#3897=CARTESIAN_POINT('Origin',(0.,-6.5,2.9));
#3898=CARTESIAN_POINT('Origin',(0.,-5.2,2.9));
#3899=CARTESIAN_POINT('',(-0.685,-3.6,2.9));
#3900=CARTESIAN_POINT('Origin',(0.,-3.6,2.9));
#3901=CARTESIAN_POINT('',(-0.685,-5.2,2.9));
#3902=CARTESIAN_POINT('Origin',(0.,-3.6,2.9));
#3903=CARTESIAN_POINT('Origin',(0.,-6.7,2.9));
#3904=CARTESIAN_POINT('',(-1.9,-6.5,2.9));
#3905=CARTESIAN_POINT('Origin',(0.,-6.5,2.9));
#3906=CARTESIAN_POINT('',(-1.9,-6.7,2.9));
#3907=CARTESIAN_POINT('',(-1.9,-6.7,2.9));
#3908=CARTESIAN_POINT('Origin',(0.,-6.7,2.9));
#3909=CARTESIAN_POINT('Origin',(0.,-6.5,2.9));
#3910=CARTESIAN_POINT('Origin',(0.,-6.7,2.9));
#3911=CARTESIAN_POINT('Origin',(-0.1,-6.8,1.9));
#3912=CARTESIAN_POINT('',(-0.1,-6.8,3.7));
#3913=CARTESIAN_POINT('',(-0.1,-6.8,1.9));
#3914=CARTESIAN_POINT('',(-0.1,-6.8,3.7));
#3915=CARTESIAN_POINT('',(-0.1,-6.7,3.7));
#3916=CARTESIAN_POINT('',(-0.1,-6.8,3.7));
#3917=CARTESIAN_POINT('',(-0.1,-6.7,1.9));
#3918=CARTESIAN_POINT('',(-0.1,-6.7,3.7));
#3919=CARTESIAN_POINT('',(-0.1,-6.8,1.9));
#3920=CARTESIAN_POINT('Origin',(0.1,-6.8,1.9));
#3921=CARTESIAN_POINT('',(0.1,-6.8,1.9));
#3922=CARTESIAN_POINT('',(-0.1,-6.8,1.9));
#3923=CARTESIAN_POINT('',(0.1,-6.7,1.9));
#3924=CARTESIAN_POINT('',(-0.1,-6.7,1.9));
#3925=CARTESIAN_POINT('',(0.1,-6.8,1.9));
#3926=CARTESIAN_POINT('Origin',(0.1,-6.8,3.7));
#3927=CARTESIAN_POINT('',(0.1,-6.8,3.7));
#3928=CARTESIAN_POINT('',(0.1,-6.8,1.9));
#3929=CARTESIAN_POINT('',(0.1,-6.7,3.7));
#3930=CARTESIAN_POINT('',(0.1,-6.7,1.9));
#3931=CARTESIAN_POINT('',(0.1,-6.8,3.7));
#3932=CARTESIAN_POINT('Origin',(0.,-6.8,4.3));
#3933=CARTESIAN_POINT('',(0.,-6.8,4.3));
#3934=CARTESIAN_POINT('',(0.1,-6.8,3.7));
#3935=CARTESIAN_POINT('',(0.,-6.7,4.3));
#3936=CARTESIAN_POINT('',(0.1,-6.7,3.7));
#3937=CARTESIAN_POINT('',(0.,-6.8,4.3));
#3938=CARTESIAN_POINT('Origin',(-0.1,-6.8,3.7));
#3939=CARTESIAN_POINT('',(0.,-6.8,4.3));
#3940=CARTESIAN_POINT('',(0.,-6.7,4.3));
#3941=CARTESIAN_POINT('Origin',(0.,-6.7,3.1));
#3942=CARTESIAN_POINT('Origin',(0.,-6.8,3.1));
#3943=CARTESIAN_POINT('',(0.,0.,0.));
#3944=CARTESIAN_POINT('Origin',(0.,-1.445,0.));
#3945=CARTESIAN_POINT('',(-0.2942,-2.9458,3.60291088309151E-17));
#3946=CARTESIAN_POINT('Origin',(0.,-2.9458,0.));
#3947=CARTESIAN_POINT('',(-0.2942,0.,-3.60291088309151E-17));
#3948=CARTESIAN_POINT('',(-0.2942,-1.445,-3.60291088309151E-17));
#3949=CARTESIAN_POINT('Origin',(0.,0.,0.));
#3950=CARTESIAN_POINT('Origin',(0.,-2.97,0.));
#3951=CARTESIAN_POINT('',(-0.24,-3.,-2.93915231795365E-17));
#3952=CARTESIAN_POINT('Origin',(0.,-3.,0.));
#3953=CARTESIAN_POINT('',(-0.27,-2.97,-3.30654635769785E-17));
#3954=CARTESIAN_POINT('Origin',(0.,-3.,0.));
#3955=CARTESIAN_POINT('Origin',(0.,0.341586508806388,0.));
#3956=CARTESIAN_POINT('',(-0.475,0.4,-5.81707229594993E-17));
#3957=CARTESIAN_POINT('Origin',(0.,0.4,0.));
#3958=CARTESIAN_POINT('',(-0.577350269189626,0.340908044531739,-7.07050159149938E-17));
#3959=CARTESIAN_POINT('',(-0.576175134594813,0.341586508806388,-7.05611034329833E-17));
#3960=CARTESIAN_POINT('',(-0.288675134594813,0.340908044531739,0.5));
#3961=CARTESIAN_POINT('Ctrl Pts',(-0.288675134594813,0.340908044531739,
0.5));
#3962=CARTESIAN_POINT('Ctrl Pts',(-0.433012701893303,0.424241377863696,
0.249999999998124));
#3963=CARTESIAN_POINT('Ctrl Pts',(-0.577350269189626,0.340908044531739,
-7.07050159149938E-17));
#3964=CARTESIAN_POINT('',(0.288675134594813,0.340908044531739,0.5));
#3965=CARTESIAN_POINT('Ctrl Pts',(0.288675134594813,0.340908044531739,0.5));
#3966=CARTESIAN_POINT('Ctrl Pts',(-2.16648921025353E-12,0.424241377863696,
0.5));
#3967=CARTESIAN_POINT('Ctrl Pts',(-0.288675134594813,0.340908044531739,
0.5));
#3968=CARTESIAN_POINT('',(0.577350269189626,0.340908044531739,0.));
#3969=CARTESIAN_POINT('Ctrl Pts',(0.577350269189626,0.340908044531739,0.));
#3970=CARTESIAN_POINT('Ctrl Pts',(0.433012701891136,0.424241377863697,0.250000000001876));
#3971=CARTESIAN_POINT('Ctrl Pts',(0.288675134594813,0.340908044531739,0.5));
#3972=CARTESIAN_POINT('',(0.288675134594813,0.340908044531739,-0.5));
#3973=CARTESIAN_POINT('Ctrl Pts',(0.288675134594813,0.340908044531739,-0.5));
#3974=CARTESIAN_POINT('Ctrl Pts',(0.433012701893303,0.424241377863696,-0.249999999998124));
#3975=CARTESIAN_POINT('Ctrl Pts',(0.577350269189626,0.340908044531739,0.));
#3976=CARTESIAN_POINT('',(-0.288675134594813,0.340908044531739,-0.5));
#3977=CARTESIAN_POINT('Ctrl Pts',(-0.288675134594813,0.340908044531739,
-0.5));
#3978=CARTESIAN_POINT('Ctrl Pts',(2.16660023255599E-12,0.424241377863696,
-0.5));
#3979=CARTESIAN_POINT('Ctrl Pts',(0.288675134594813,0.340908044531739,-0.5));
#3980=CARTESIAN_POINT('Ctrl Pts',(-0.577350269189626,0.340908044531739,
-7.07050159149938E-17));
#3981=CARTESIAN_POINT('Ctrl Pts',(-0.433012701891136,0.424241377863697,
-0.250000000001876));
#3982=CARTESIAN_POINT('Ctrl Pts',(-0.288675134594813,0.340908044531739,
-0.5));
#3983=CARTESIAN_POINT('Origin',(0.288675134594813,0.,-0.5));
#3984=CARTESIAN_POINT('',(0.288675134594813,0.,-0.5));
#3985=CARTESIAN_POINT('',(0.288675134594813,0.,-0.5));
#3986=CARTESIAN_POINT('',(-0.288675134594813,0.,-0.5));
#3987=CARTESIAN_POINT('',(0.288675134594813,0.,-0.5));
#3988=CARTESIAN_POINT('',(-0.288675134594813,0.,-0.5));
#3989=CARTESIAN_POINT('Origin',(0.577350269189626,0.,0.));
#3990=CARTESIAN_POINT('',(0.577350269189626,0.,0.));
#3991=CARTESIAN_POINT('',(0.577350269189626,0.,0.));
#3992=CARTESIAN_POINT('',(0.577350269189626,0.,0.));
#3993=CARTESIAN_POINT('Origin',(0.288675134594813,0.,0.5));
#3994=CARTESIAN_POINT('',(0.288675134594813,0.,0.5));
#3995=CARTESIAN_POINT('',(0.288675134594813,0.,0.5));
#3996=CARTESIAN_POINT('',(0.288675134594813,0.,0.5));
#3997=CARTESIAN_POINT('Origin',(-0.288675134594813,0.,0.5));
#3998=CARTESIAN_POINT('',(-0.288675134594813,0.,0.5));
#3999=CARTESIAN_POINT('',(-0.288675134594813,0.,0.5));
#4000=CARTESIAN_POINT('',(-0.288675134594813,0.,0.5));
#4001=CARTESIAN_POINT('Origin',(-0.577350269189626,0.,-7.07050159149938E-17));
#4002=CARTESIAN_POINT('',(-0.577350269189626,0.,-7.07050159149938E-17));
#4003=CARTESIAN_POINT('',(-0.577350269189626,0.,-7.07050159149938E-17));
#4004=CARTESIAN_POINT('',(-0.577350269189626,0.,-7.07050159149938E-17));
#4005=CARTESIAN_POINT('Origin',(-0.288675134594813,0.,-0.5));
#4006=CARTESIAN_POINT('',(-0.288675134594813,0.,-0.5));
#4007=CARTESIAN_POINT('Origin',(0.,0.4,0.));
#4008=CARTESIAN_POINT('Origin',(0.,0.,0.));
#4009=CARTESIAN_POINT('',(0.,0.,0.));
#4010=CARTESIAN_POINT('',(0.,0.,0.));
#4011=CARTESIAN_POINT('',(0.,0.,0.));
#4012=CARTESIAN_POINT('',(-3.85,0.,6.));
#4013=CARTESIAN_POINT('',(3.85,0.,8.5));
#4014=CARTESIAN_POINT('',(0.,-0.8,0.));
#4015=CARTESIAN_POINT('',(0.,0.,9.8));
#4016=CARTESIAN_POINT('',(8.,3.7,5.6));
#4017=CARTESIAN_POINT('',(-1.5,-1.4,4.2));
#4018=CARTESIAN_POINT('',(-1.5,1.4,4.2));
#4019=CARTESIAN_POINT('',(1.5,-1.4,4.2));
#4020=CARTESIAN_POINT('',(1.5,1.4,4.2));
#4021=CARTESIAN_POINT('',(0.,0.,0.));
#4022=UNCERTAINTY_MEASURE_WITH_UNIT(LENGTH_MEASURE(0.001),#4044,
'DISTANCE_ACCURACY_VALUE',
'Maximum model space distance between geometric entities at asserted c
onnectivities');
#4023=UNCERTAINTY_MEASURE_WITH_UNIT(LENGTH_MEASURE(0.001),#4044,
'DISTANCE_ACCURACY_VALUE',
'Maximum model space distance between geometric entities at asserted c
onnectivities');
#4024=UNCERTAINTY_MEASURE_WITH_UNIT(LENGTH_MEASURE(0.001),#4044,
'DISTANCE_ACCURACY_VALUE',
'Maximum model space distance between geometric entities at asserted c
onnectivities');
#4025=UNCERTAINTY_MEASURE_WITH_UNIT(LENGTH_MEASURE(0.001),#4044,
'DISTANCE_ACCURACY_VALUE',
'Maximum model space distance between geometric entities at asserted c
onnectivities');
#4026=UNCERTAINTY_MEASURE_WITH_UNIT(LENGTH_MEASURE(0.001),#4044,
'DISTANCE_ACCURACY_VALUE',
'Maximum model space distance between geometric entities at asserted c
onnectivities');
#4027=UNCERTAINTY_MEASURE_WITH_UNIT(LENGTH_MEASURE(0.001),#4044,
'DISTANCE_ACCURACY_VALUE',
'Maximum model space distance between geometric entities at asserted c
onnectivities');
#4028=UNCERTAINTY_MEASURE_WITH_UNIT(LENGTH_MEASURE(0.001),#4044,
'DISTANCE_ACCURACY_VALUE',
'Maximum model space distance between geometric entities at asserted c
onnectivities');
#4029=UNCERTAINTY_MEASURE_WITH_UNIT(LENGTH_MEASURE(0.001),#4044,
'DISTANCE_ACCURACY_VALUE',
'Maximum model space distance between geometric entities at asserted c
onnectivities');
#4030=UNCERTAINTY_MEASURE_WITH_UNIT(LENGTH_MEASURE(0.001),#4044,
'DISTANCE_ACCURACY_VALUE',
'Maximum model space distance between geometric entities at asserted c
onnectivities');
#4031=UNCERTAINTY_MEASURE_WITH_UNIT(LENGTH_MEASURE(0.001),#4044,
'DISTANCE_ACCURACY_VALUE',
'Maximum model space distance between geometric entities at asserted c
onnectivities');
#4032=UNCERTAINTY_MEASURE_WITH_UNIT(LENGTH_MEASURE(0.001),#4044,
'DISTANCE_ACCURACY_VALUE',
'Maximum model space distance between geometric entities at asserted c
onnectivities');
#4033=(
GEOMETRIC_REPRESENTATION_CONTEXT(3)
GLOBAL_UNCERTAINTY_ASSIGNED_CONTEXT((#4022))
GLOBAL_UNIT_ASSIGNED_CONTEXT((#4044,#4046,#4047))
REPRESENTATION_CONTEXT('','3D')
);
#4034=(
GEOMETRIC_REPRESENTATION_CONTEXT(3)
GLOBAL_UNCERTAINTY_ASSIGNED_CONTEXT((#4023))
GLOBAL_UNIT_ASSIGNED_CONTEXT((#4044,#4046,#4047))
REPRESENTATION_CONTEXT('','3D')
);
#4035=(
GEOMETRIC_REPRESENTATION_CONTEXT(3)
GLOBAL_UNCERTAINTY_ASSIGNED_CONTEXT((#4024))
GLOBAL_UNIT_ASSIGNED_CONTEXT((#4044,#4046,#4047))
REPRESENTATION_CONTEXT('','3D')
);
#4036=(
GEOMETRIC_REPRESENTATION_CONTEXT(3)
GLOBAL_UNCERTAINTY_ASSIGNED_CONTEXT((#4025))
GLOBAL_UNIT_ASSIGNED_CONTEXT((#4044,#4046,#4047))
REPRESENTATION_CONTEXT('','3D')
);
#4037=(
GEOMETRIC_REPRESENTATION_CONTEXT(3)
GLOBAL_UNCERTAINTY_ASSIGNED_CONTEXT((#4026))
GLOBAL_UNIT_ASSIGNED_CONTEXT((#4044,#4046,#4047))
REPRESENTATION_CONTEXT('','3D')
);
#4038=(
GEOMETRIC_REPRESENTATION_CONTEXT(3)
GLOBAL_UNCERTAINTY_ASSIGNED_CONTEXT((#4027))
GLOBAL_UNIT_ASSIGNED_CONTEXT((#4044,#4046,#4047))
REPRESENTATION_CONTEXT('','3D')
);
#4039=(
GEOMETRIC_REPRESENTATION_CONTEXT(3)
GLOBAL_UNCERTAINTY_ASSIGNED_CONTEXT((#4028))
GLOBAL_UNIT_ASSIGNED_CONTEXT((#4044,#4046,#4047))
REPRESENTATION_CONTEXT('','3D')
);
#4040=(
GEOMETRIC_REPRESENTATION_CONTEXT(3)
GLOBAL_UNCERTAINTY_ASSIGNED_CONTEXT((#4029))
GLOBAL_UNIT_ASSIGNED_CONTEXT((#4044,#4046,#4047))
REPRESENTATION_CONTEXT('','3D')
);
#4041=(
GEOMETRIC_REPRESENTATION_CONTEXT(3)
GLOBAL_UNCERTAINTY_ASSIGNED_CONTEXT((#4030))
GLOBAL_UNIT_ASSIGNED_CONTEXT((#4044,#4046,#4047))
REPRESENTATION_CONTEXT('','3D')
);
#4042=(
GEOMETRIC_REPRESENTATION_CONTEXT(3)
GLOBAL_UNCERTAINTY_ASSIGNED_CONTEXT((#4031))
GLOBAL_UNIT_ASSIGNED_CONTEXT((#4044,#4046,#4047))
REPRESENTATION_CONTEXT('','3D')
);
#4043=(
GEOMETRIC_REPRESENTATION_CONTEXT(3)
GLOBAL_UNCERTAINTY_ASSIGNED_CONTEXT((#4032))
GLOBAL_UNIT_ASSIGNED_CONTEXT((#4044,#4046,#4047))
REPRESENTATION_CONTEXT('','3D')
);
#4044=(
LENGTH_UNIT()
NAMED_UNIT(*)
SI_UNIT(.CENTI.,.METRE.)
);
#4045=(
LENGTH_UNIT()
NAMED_UNIT(*)
SI_UNIT($,.METRE.)
);
#4046=(
NAMED_UNIT(*)
PLANE_ANGLE_UNIT()
SI_UNIT($,.RADIAN.)
);
#4047=(
NAMED_UNIT(*)
SI_UNIT($,.STERADIAN.)
SOLID_ANGLE_UNIT()
);
#4048=SHAPE_DEFINITION_REPRESENTATION(#4058,#4081);
#4049=SHAPE_DEFINITION_REPRESENTATION(#4059,#4082);
#4050=SHAPE_DEFINITION_REPRESENTATION(#4060,#4083);
#4051=SHAPE_DEFINITION_REPRESENTATION(#4061,#4084);
#4052=SHAPE_DEFINITION_REPRESENTATION(#4062,#4085);
#4053=SHAPE_DEFINITION_REPRESENTATION(#4063,#4086);
#4054=SHAPE_DEFINITION_REPRESENTATION(#4064,#4087);
#4055=SHAPE_DEFINITION_REPRESENTATION(#4065,#4088);
#4056=SHAPE_DEFINITION_REPRESENTATION(#4066,#4089);
#4057=SHAPE_DEFINITION_REPRESENTATION(#4067,#4090);
#4058=PRODUCT_DEFINITION_SHAPE('',$,#4092);
#4059=PRODUCT_DEFINITION_SHAPE('',$,#4093);
#4060=PRODUCT_DEFINITION_SHAPE('',$,#4094);
#4061=PRODUCT_DEFINITION_SHAPE('',$,#4095);
#4062=PRODUCT_DEFINITION_SHAPE('',$,#4096);
#4063=PRODUCT_DEFINITION_SHAPE('',$,#4097);
#4064=PRODUCT_DEFINITION_SHAPE('',$,#4098);
#4065=PRODUCT_DEFINITION_SHAPE('',$,#4099);
#4066=PRODUCT_DEFINITION_SHAPE('',$,#4100);
#4067=PRODUCT_DEFINITION_SHAPE('',$,#4101);
#4068=PRODUCT_DEFINITION_SHAPE($,$,#50);
#4069=PRODUCT_DEFINITION_SHAPE($,$,#51);
#4070=PRODUCT_DEFINITION_SHAPE($,$,#52);
#4071=PRODUCT_DEFINITION_SHAPE($,$,#53);
#4072=PRODUCT_DEFINITION_SHAPE($,$,#54);
#4073=PRODUCT_DEFINITION_SHAPE($,$,#55);
#4074=PRODUCT_DEFINITION_SHAPE($,$,#56);
#4075=PRODUCT_DEFINITION_SHAPE($,$,#57);
#4076=PRODUCT_DEFINITION_SHAPE($,$,#58);
#4077=PRODUCT_DEFINITION_SHAPE($,$,#59);
#4078=PRODUCT_DEFINITION_SHAPE($,$,#60);
#4079=PRODUCT_DEFINITION_SHAPE($,$,#61);
#4080=PRODUCT_DEFINITION_SHAPE($,$,#62);
#4081=SHAPE_REPRESENTATION('',(#2308,#2558),#4033);
#4082=SHAPE_REPRESENTATION('',(#2309,#2546,#2547,#2548,#2549,#2550,#2551,
#2552,#2553,#2554,#2555,#2556,#2557),#4034);
#4083=SHAPE_REPRESENTATION('',(#2310),#4035);
#4084=SHAPE_REPRESENTATION('',(#2379),#4036);
#4085=SHAPE_REPRESENTATION('',(#2400),#4037);
#4086=SHAPE_REPRESENTATION('',(#2467),#4038);
#4087=SHAPE_REPRESENTATION('',(#2491),#4039);
#4088=SHAPE_REPRESENTATION('',(#2503),#4040);
#4089=SHAPE_REPRESENTATION('',(#2507),#4041);
#4090=SHAPE_REPRESENTATION('',(#2529),#4042);
#4091=PRODUCT_DEFINITION_CONTEXT('part definition',#4123,'design');
#4092=PRODUCT_DEFINITION('PAT-045',
'PAT-045',#4102,#4091);
#4093=PRODUCT_DEFINITION(
'Guage isolation set','Guage isolation set',
#4103,#4091);
#4094=PRODUCT_DEFINITION('Gauge isolation valve body',
'Gauge isolation valve body',#4104,#4091);
#4095=PRODUCT_DEFINITION('Restrictor and gauge adapter',
'Restrictor and gauge adapter',#4105,#4091);
#4096=PRODUCT_DEFINITION('Valve mounting saddle',
'Valve mounting saddle',#4106,#4091);
#4097=PRODUCT_DEFINITION(
'Hex Pipe Nipple - 1-2 Inch Tapered Pipe Thread',
'Hex Pipe Nipple - 1-2 Inch Tapered Pipe Thread',#4107,#4091);
#4098=PRODUCT_DEFINITION('Metering needle and grip',
'Metering needle and grip',#4108,#4091);
#4099=PRODUCT_DEFINITION('O-Ring','O-Ring',#4109,#4091);
#4100=PRODUCT_DEFINITION('Gauge dummy','Gauge dummy',#4110,#4091);
#4101=PRODUCT_DEFINITION('Hex Bolt - M6 x 30 mm',
'Hex Bolt - M6 x 30 mm',#4111,#4091);
#4102=PRODUCT_DEFINITION_FORMATION('',$,#4125);
#4103=PRODUCT_DEFINITION_FORMATION('',$,#4126);
#4104=PRODUCT_DEFINITION_FORMATION('',$,#4127);
#4105=PRODUCT_DEFINITION_FORMATION('',$,#4128);
#4106=PRODUCT_DEFINITION_FORMATION('',$,#4129);
#4107=PRODUCT_DEFINITION_FORMATION('',$,#4130);
#4108=PRODUCT_DEFINITION_FORMATION('',$,#4131);
#4109=PRODUCT_DEFINITION_FORMATION('',$,#4132);
#4110=PRODUCT_DEFINITION_FORMATION('',$,#4133);
#4111=PRODUCT_DEFINITION_FORMATION('',$,#4134);
#4112=PRODUCT_RELATED_PRODUCT_CATEGORY('PAT-045',
'PAT-045',(#4125));
#4113=PRODUCT_RELATED_PRODUCT_CATEGORY('Guage isolation set',
'Guage isolation set',(#4126));
#4114=PRODUCT_RELATED_PRODUCT_CATEGORY('Gauge isolation valve body',
'Gauge isolation valve body',(#4127));
#4115=PRODUCT_RELATED_PRODUCT_CATEGORY('Restrictor and gauge adapter',
'Restrictor and gauge adapter',(#4128));
#4116=PRODUCT_RELATED_PRODUCT_CATEGORY('Valve mounting saddle',
'Valve mounting saddle',(#4129));
#4117=PRODUCT_RELATED_PRODUCT_CATEGORY(
'Hex Pipe Nipple - 1-2 Inch Tapered Pipe Thread',
'Hex Pipe Nipple - 1-2 Inch Tapered Pipe Thread',(#4130));
#4118=PRODUCT_RELATED_PRODUCT_CATEGORY('Metering needle and grip',
'Metering needle and grip',(#4131));
#4119=PRODUCT_RELATED_PRODUCT_CATEGORY('O-Ring','O-Ring',(#4132));
#4120=PRODUCT_RELATED_PRODUCT_CATEGORY('Gauge dummy','Gauge dummy',(#4133));
#4121=PRODUCT_RELATED_PRODUCT_CATEGORY('Hex Bolt - M6 x 30 mm',
'Hex Bolt - M6 x 30 mm',(#4134));
#4122=APPLICATION_PROTOCOL_DEFINITION('international standard',
'automotive_design',2009,#4123);
#4123=APPLICATION_CONTEXT(
'Core Data for Automotive Mechanical Design Process');
#4124=PRODUCT_CONTEXT('part definition',#4123,'mechanical');
#4125=PRODUCT('PAT-045',
'PAT-045','PAT-045',(#4124));
#4126=PRODUCT('Guage isolation set',
'Guage isolation set','Guage isolation set',
(#4124));
#4127=PRODUCT('Gauge isolation valve body','Gauge isolation valve body',
'Gauge isolation valve body',(#4124));
#4128=PRODUCT('Restrictor and gauge adapter',
'Restrictor and gauge adapter','Restrictor and gauge adapter',(#4124));
#4129=PRODUCT('Valve mounting saddle','Valve mounting saddle',
'Valve mounting saddle',(#4124));
#4130=PRODUCT('Hex Pipe Nipple - 1-2 Inch Tapered Pipe Thread',
'Hex Pipe Nipple - 1-2 Inch Tapered Pipe Thread',
'Hex Pipe Nipple - 1-2 Inch Tapered Pipe Thread',(#4124));
#4131=PRODUCT('Metering needle and grip','Metering needle and grip',
'Metering needle and grip',(#4124));
#4132=PRODUCT('O-Ring','O-Ring','O-Ring',(#4124));
#4133=PRODUCT('Gauge dummy','Gauge dummy','Gauge dummy',(#4124));
#4134=PRODUCT('Hex Bolt - M6 x 30 mm','Hex Bolt - M6 x 30 mm',
'Hex Bolt - M6 x 30 mm',(#4124));
#4135=PRESENTATION_STYLE_ASSIGNMENT((#4140));
#4136=PRESENTATION_STYLE_ASSIGNMENT((#4141));
#4137=PRESENTATION_STYLE_ASSIGNMENT((#4142));
#4138=PRESENTATION_STYLE_ASSIGNMENT((#4143));
#4139=PRESENTATION_STYLE_ASSIGNMENT((#4144));
#4140=SURFACE_STYLE_USAGE(.BOTH.,#4145);
#4141=SURFACE_STYLE_USAGE(.BOTH.,#4146);
#4142=SURFACE_STYLE_USAGE(.BOTH.,#4147);
#4143=SURFACE_STYLE_USAGE(.BOTH.,#4148);
#4144=SURFACE_STYLE_USAGE(.BOTH.,#4149);
#4145=SURFACE_SIDE_STYLE('',(#4150));
#4146=SURFACE_SIDE_STYLE('',(#4151));
#4147=SURFACE_SIDE_STYLE('',(#4152));
#4148=SURFACE_SIDE_STYLE('',(#4153));
#4149=SURFACE_SIDE_STYLE('',(#4154));
#4150=SURFACE_STYLE_FILL_AREA(#4155);
#4151=SURFACE_STYLE_FILL_AREA(#4156);
#4152=SURFACE_STYLE_FILL_AREA(#4157);
#4153=SURFACE_STYLE_FILL_AREA(#4158);
#4154=SURFACE_STYLE_FILL_AREA(#4159);
#4155=FILL_AREA_STYLE('Steel - Satin',(#4160));
#4156=FILL_AREA_STYLE('CAD Library Painted - Engineering blue',(#4161));
#4157=FILL_AREA_STYLE('CAD Library Painted - Steel gray',(#4162));
#4158=FILL_AREA_STYLE('CAD Library Painted - Graphite',(#4163));
#4159=FILL_AREA_STYLE('CAD Library Painted - Off white',(#4164));
#4160=FILL_AREA_STYLE_COLOUR('Steel - Satin',#4165);
#4161=FILL_AREA_STYLE_COLOUR('CAD Library Painted - Engineering blue',#4166);
#4162=FILL_AREA_STYLE_COLOUR('CAD Library Painted - Steel gray',#4167);
#4163=FILL_AREA_STYLE_COLOUR('CAD Library Painted - Graphite',#4168);
#4164=FILL_AREA_STYLE_COLOUR('CAD Library Painted - Off white',#4169);
#4165=COLOUR_RGB('Steel - Satin',0.627450980392157,0.627450980392157,0.627450980392157);
#4166=COLOUR_RGB('CAD Library Painted - Engineering blue',0.12156862745098,
0.356862745098039,0.6);
#4167=COLOUR_RGB('CAD Library Painted - Steel gray',0.592156862745098,0.631372549019608,
0.67843137254902);
#4168=COLOUR_RGB('CAD Library Painted - Graphite',0.0980392156862745,0.109803921568627,
0.125490196078431);
#4169=COLOUR_RGB('CAD Library Painted - Off white',0.909803921568627,0.901960784313726,
0.858823529411765);
#4170=COLOUR_RGB('Dark Blue',0.08,0.2,0.34);
#4171=FILL_AREA_STYLE_COLOUR('',#4170);
#4172=FILL_AREA_STYLE('',(#4171));
#4173=SURFACE_STYLE_FILL_AREA(#4172);
#4174=SURFACE_SIDE_STYLE('',(#4173));
#4175=SURFACE_STYLE_USAGE(.BOTH.,#4174);
#4176=PRESENTATION_STYLE_ASSIGNMENT((#4175));
#4177=COLOUR_RGB('Light Blue',0.38,0.62,0.78);
#4178=FILL_AREA_STYLE_COLOUR('',#4177);
#4179=FILL_AREA_STYLE('',(#4178));
#4180=SURFACE_STYLE_FILL_AREA(#4179);
#4181=SURFACE_SIDE_STYLE('',(#4180));
#4182=SURFACE_STYLE_USAGE(.BOTH.,#4181);
#4183=PRESENTATION_STYLE_ASSIGNMENT((#4182));
#4184=COLOUR_RGB('Sky Blue',0.24,0.69,0.87);
#4185=FILL_AREA_STYLE_COLOUR('',#4184);
#4186=FILL_AREA_STYLE('',(#4185));
#4187=SURFACE_STYLE_FILL_AREA(#4186);
#4188=SURFACE_SIDE_STYLE('',(#4187));
#4189=SURFACE_STYLE_USAGE(.BOTH.,#4188);
#4190=PRESENTATION_STYLE_ASSIGNMENT((#4189));
#4191=COLOUR_RGB('Grey',0.48,0.52,0.57);
#4192=FILL_AREA_STYLE_COLOUR('',#4191);
#4193=FILL_AREA_STYLE('',(#4192));
#4194=SURFACE_STYLE_FILL_AREA(#4193);
#4195=SURFACE_SIDE_STYLE('',(#4194));
#4196=SURFACE_STYLE_USAGE(.BOTH.,#4195);
#4197=PRESENTATION_STYLE_ASSIGNMENT((#4196));
#4198=COLOUR_RGB('Black',0.12,0.14,0.17);
#4199=FILL_AREA_STYLE_COLOUR('',#4198);
#4200=FILL_AREA_STYLE('',(#4199));
#4201=SURFACE_STYLE_FILL_AREA(#4200);
#4202=SURFACE_SIDE_STYLE('',(#4201));
#4203=SURFACE_STYLE_USAGE(.BOTH.,#4202);
#4204=PRESENTATION_STYLE_ASSIGNMENT((#4203));
#4205=COLOUR_RGB('Off White',0.89,0.88,0.83);
#4206=FILL_AREA_STYLE_COLOUR('',#4205);
#4207=FILL_AREA_STYLE('',(#4206));
#4208=SURFACE_STYLE_FILL_AREA(#4207);
#4209=SURFACE_SIDE_STYLE('',(#4208));
#4210=SURFACE_STYLE_USAGE(.BOTH.,#4209);
#4211=PRESENTATION_STYLE_ASSIGNMENT((#4210));
ENDSEC;
END-ISO-10303-21;
